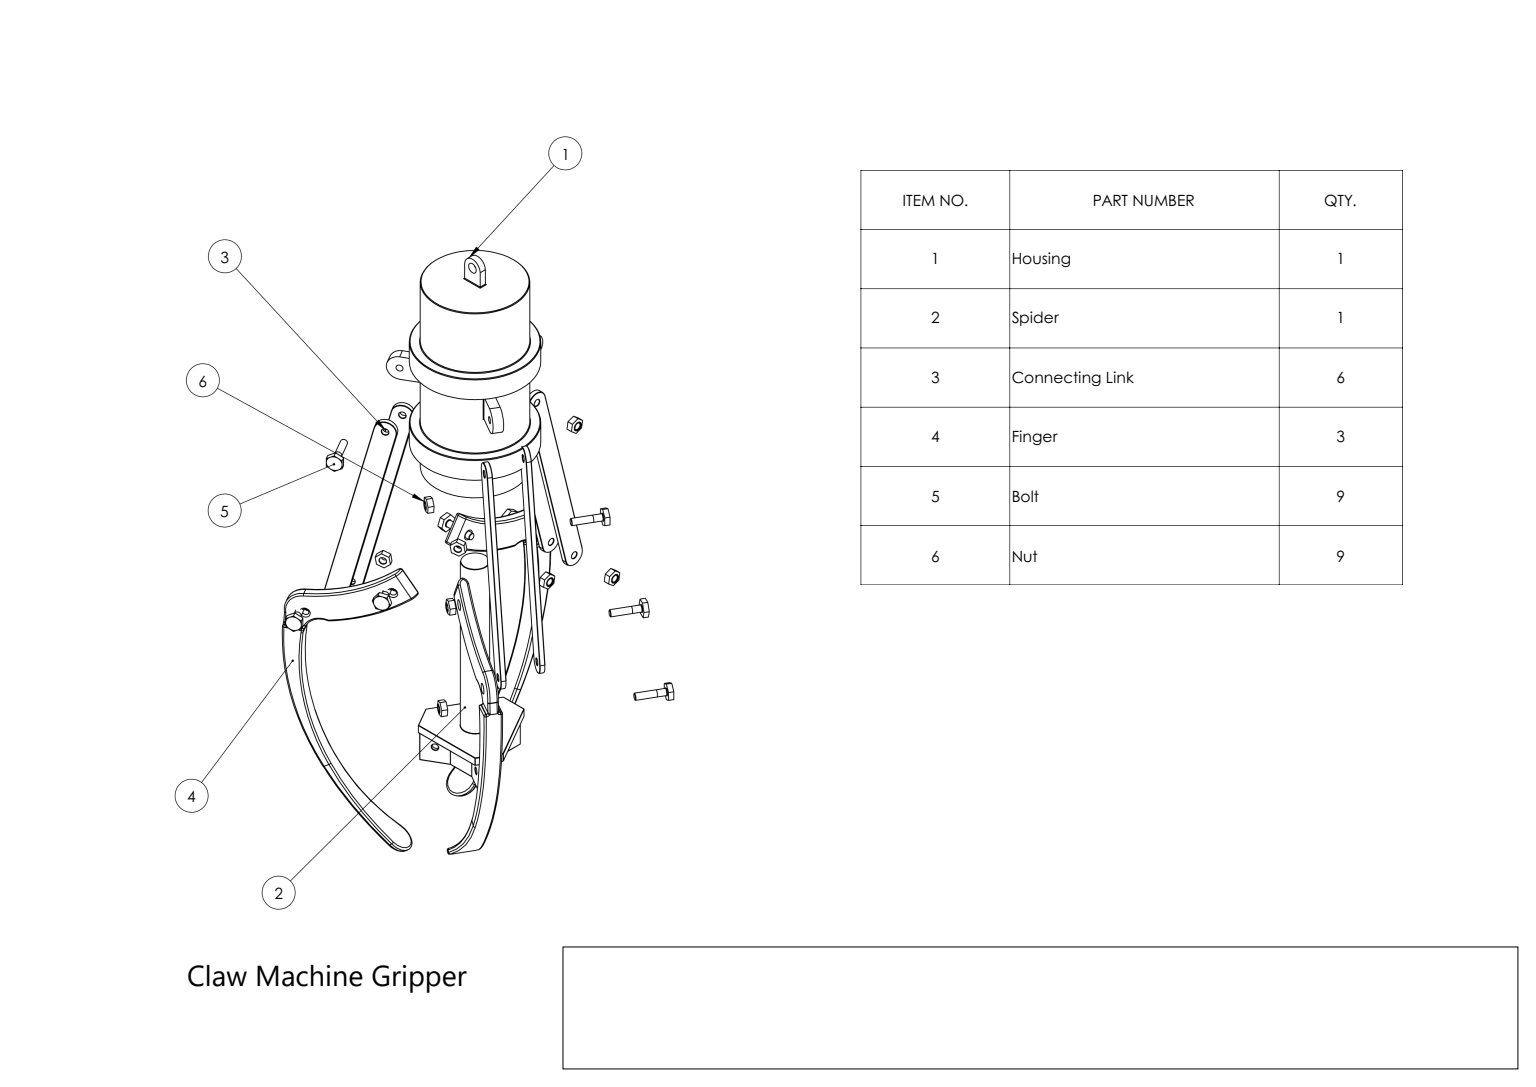
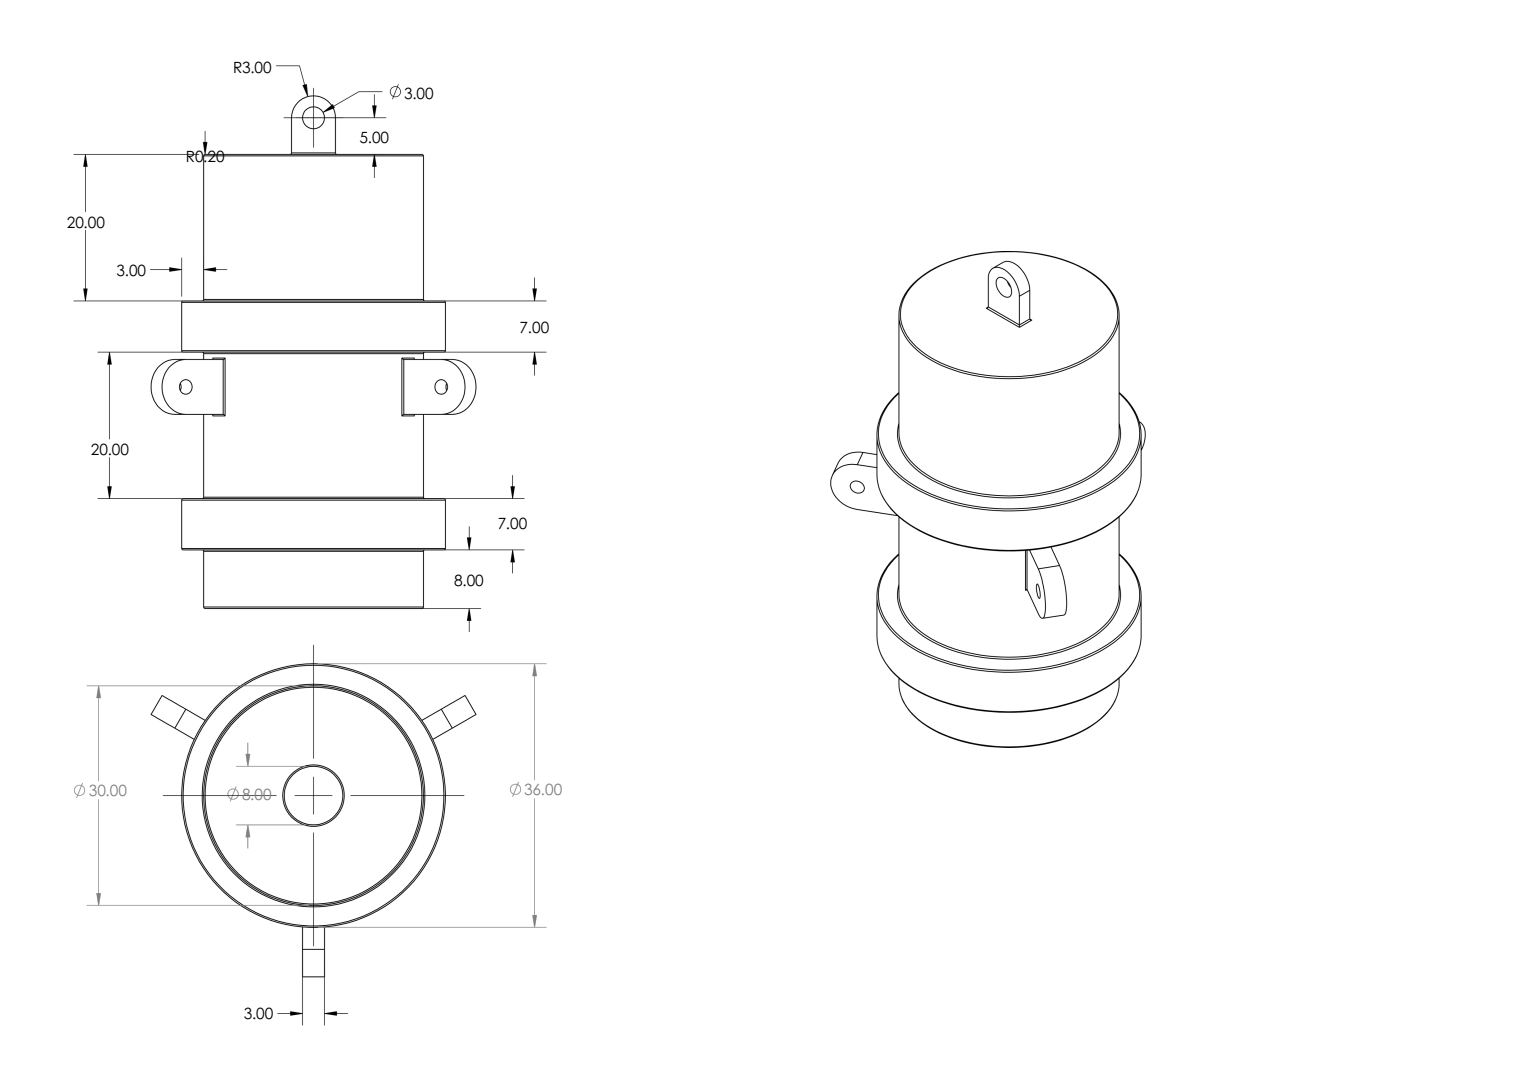
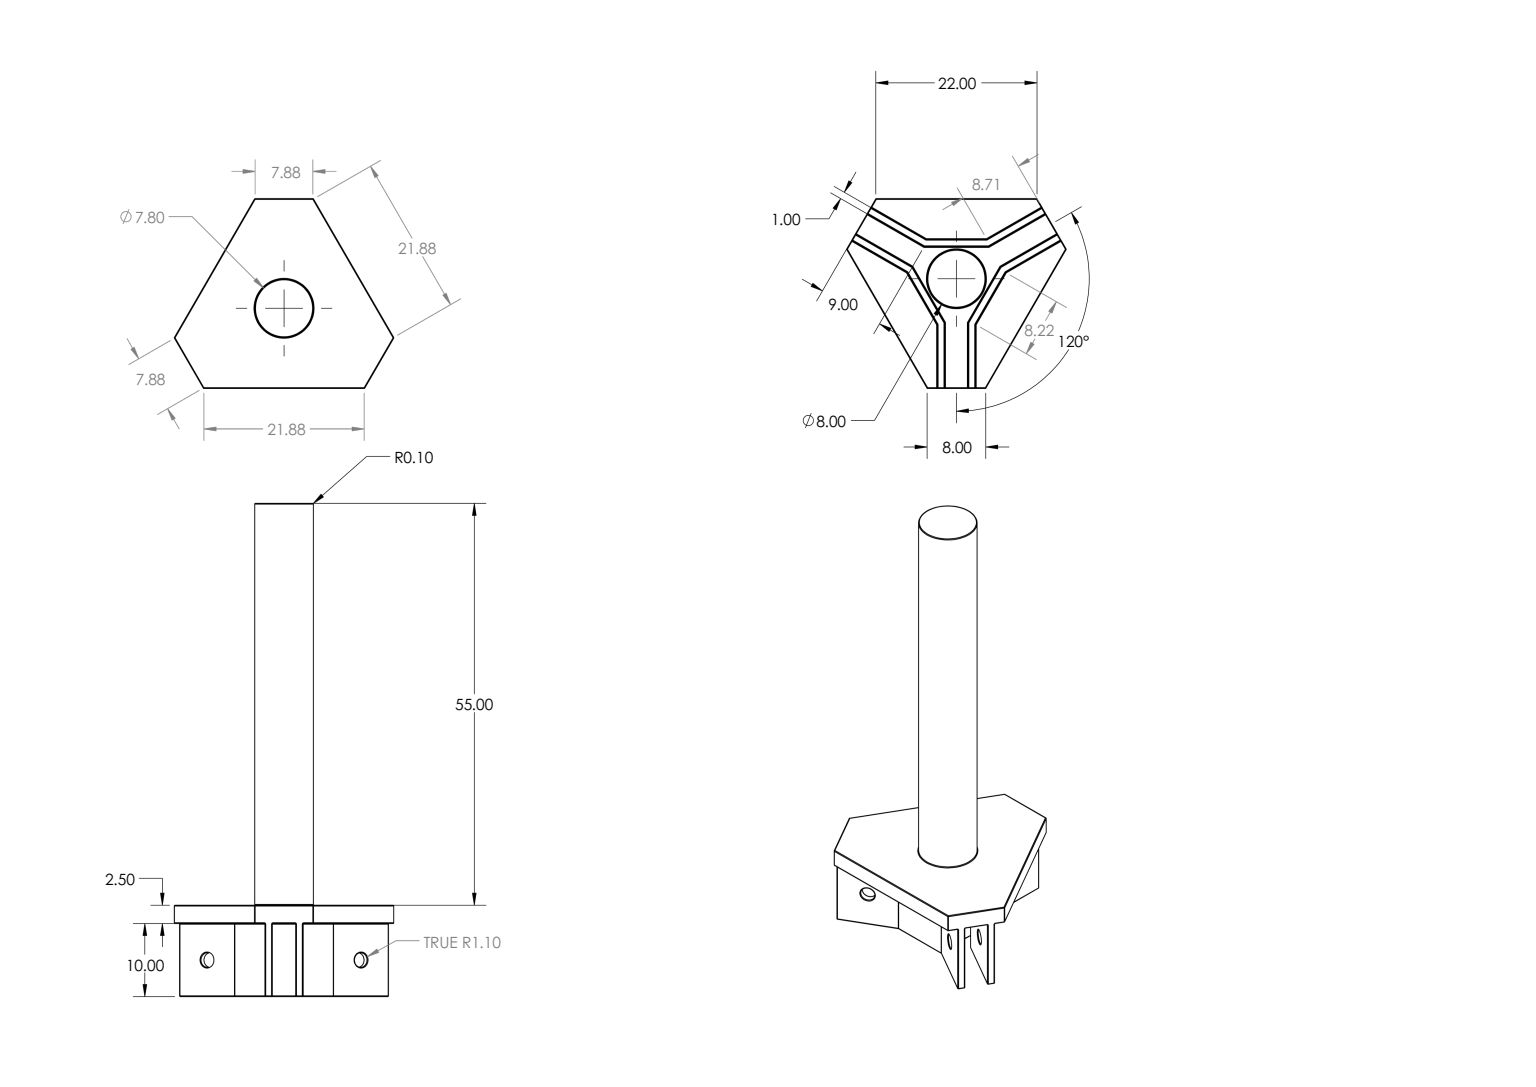
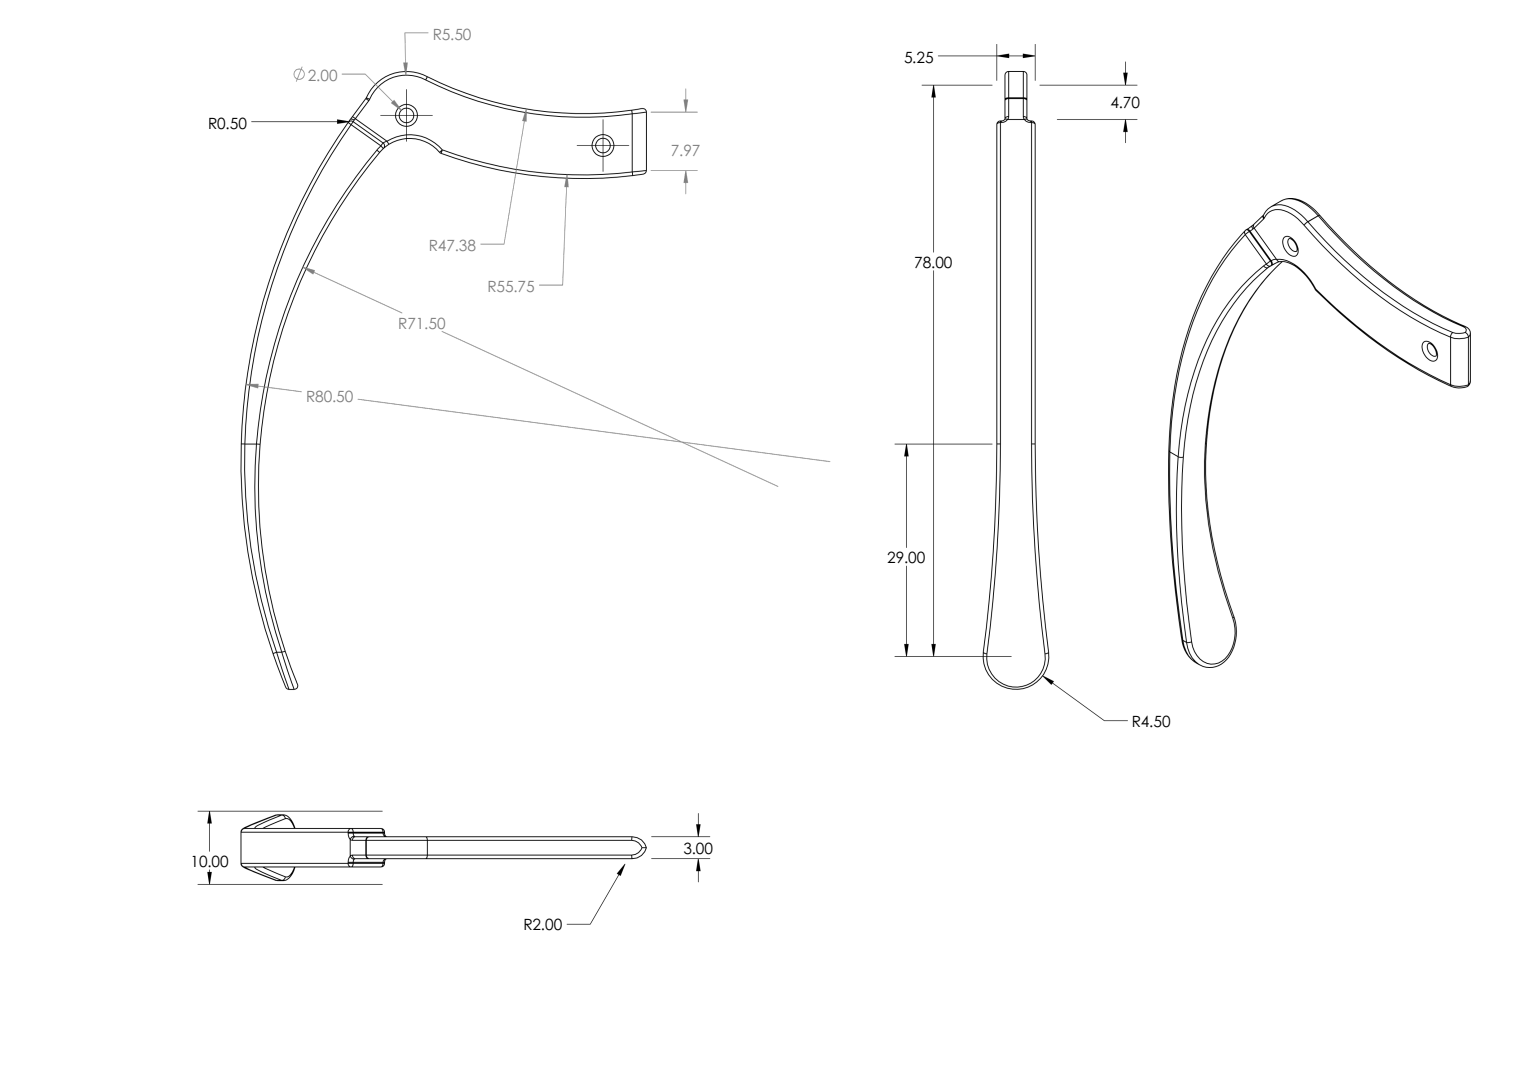
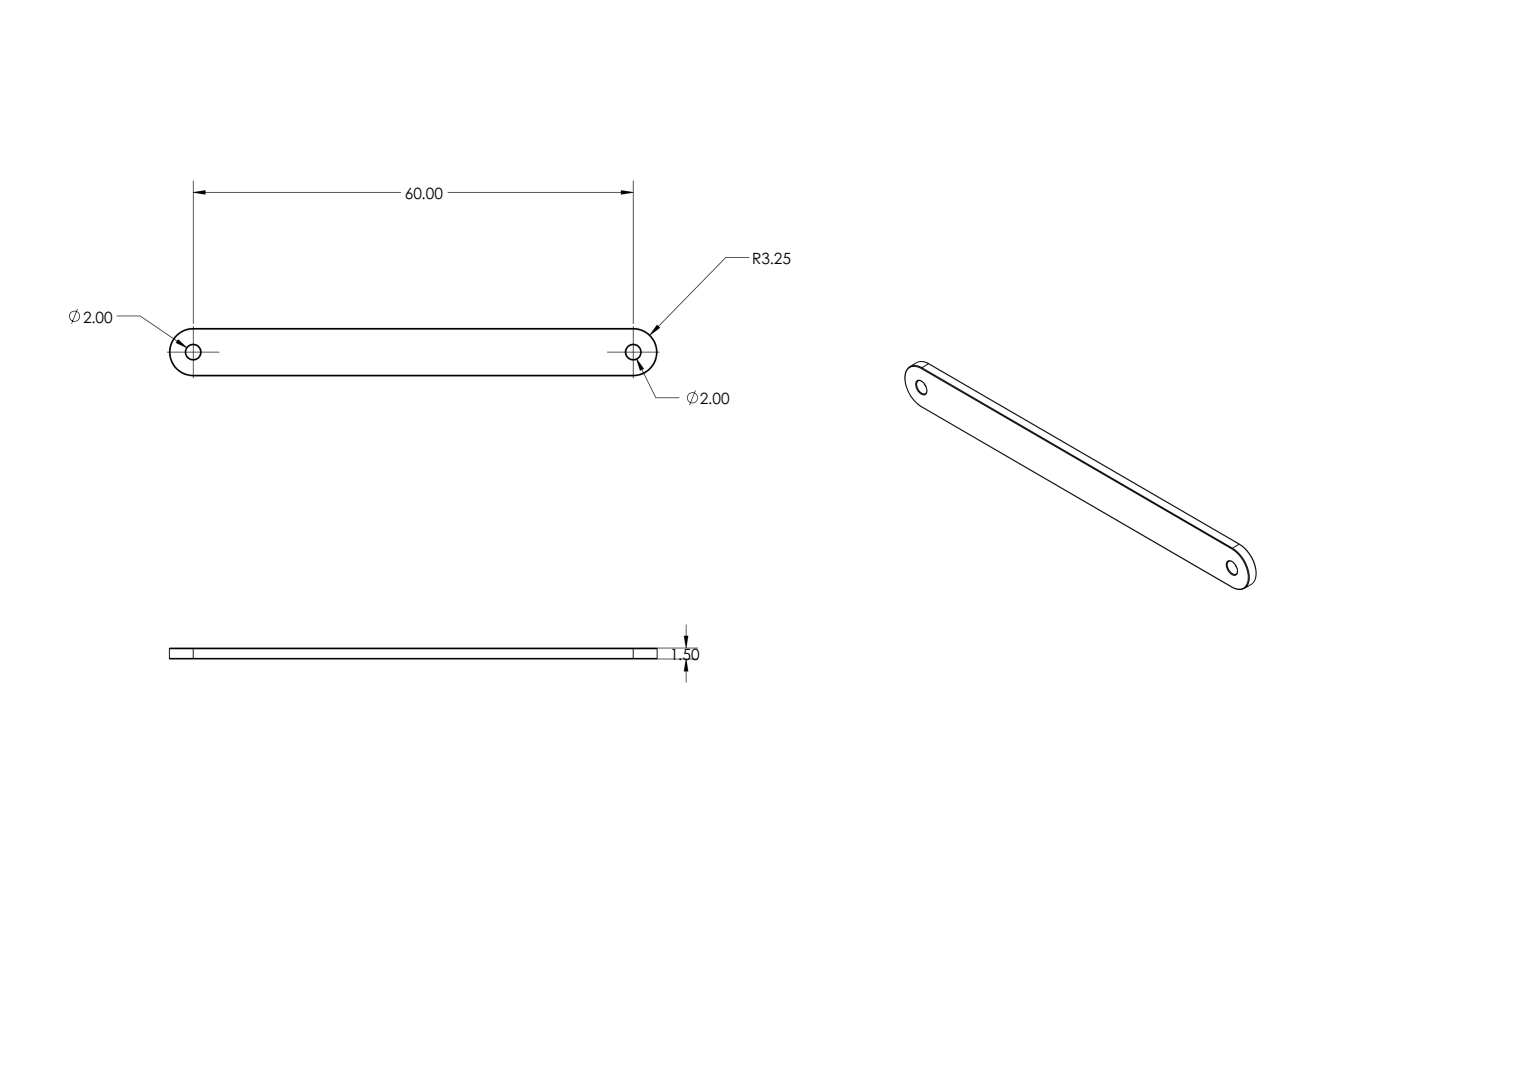
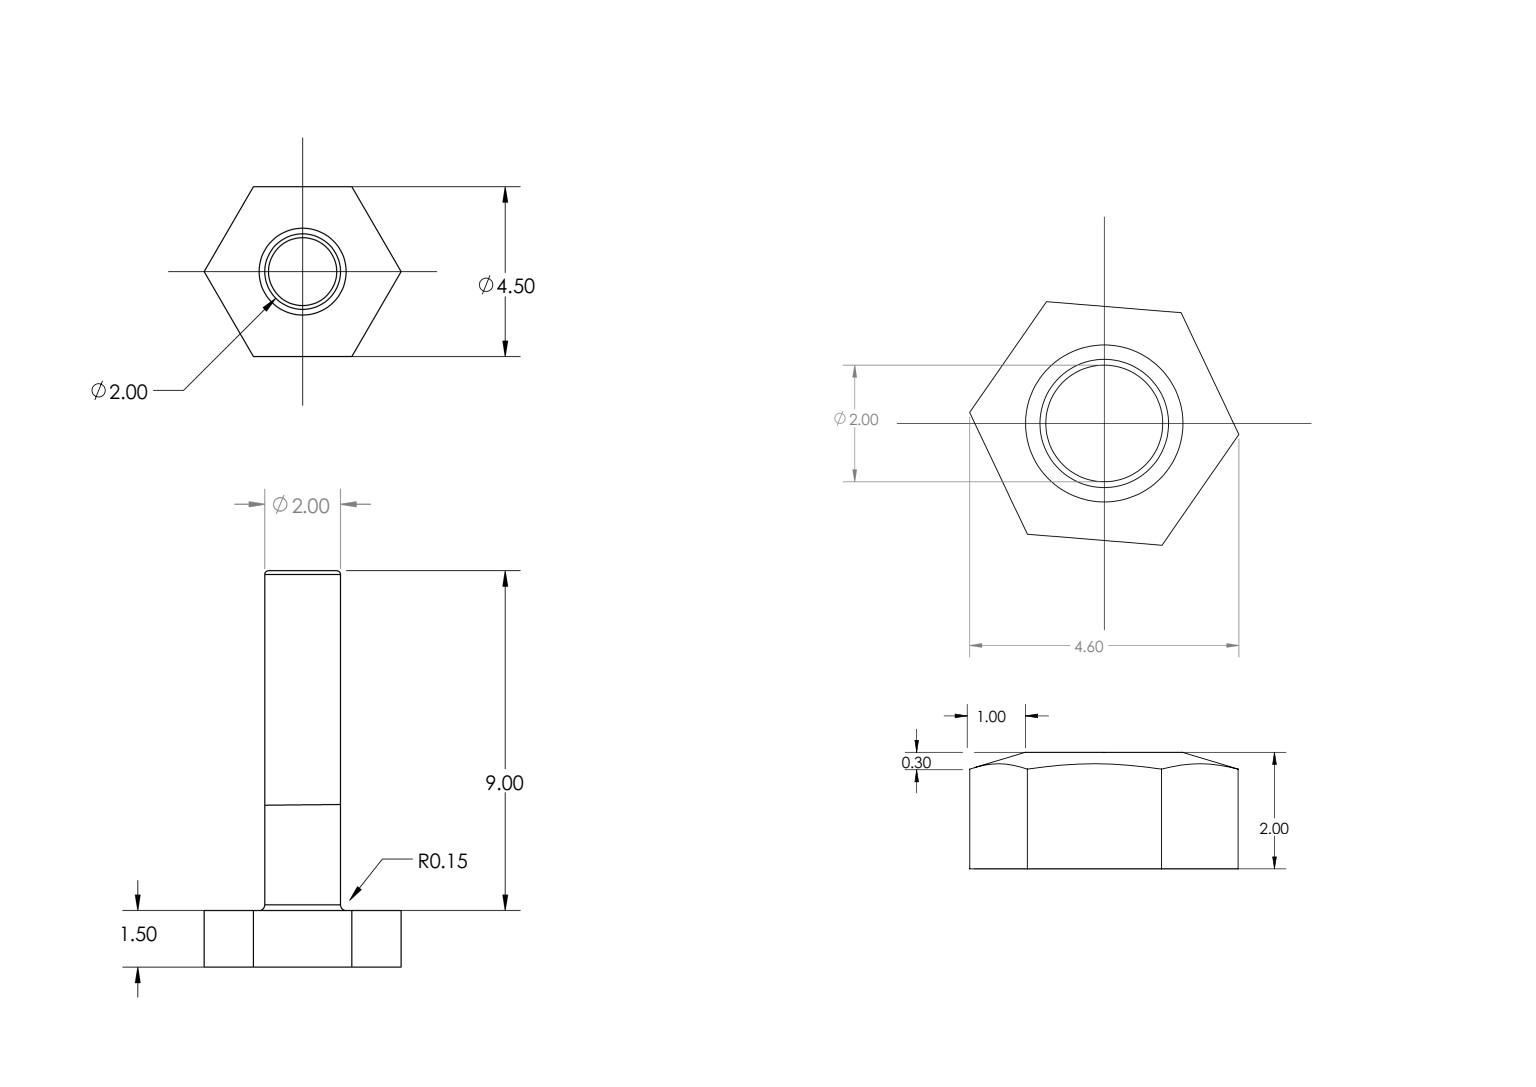
ISO-10303-21;
HEADER;
FILE_DESCRIPTION (('STEP AP214'),
    '1' );
FILE_NAME ('MAT-022',
    '2026-10-24T18:16:00',
    ( '' ),
    ( '' ),
    'SwSTEP 2.0',
    'SolidWorks 2025',
    '' );
FILE_SCHEMA (( 'AUTOMOTIVE_DESIGN' ));
ENDSEC;

DATA;
#1 = CARTESIAN_POINT ( 'NONE',  ( -1.293236445124221312, 0.1355266887446167634, -0.03937007874015747977 ) ) ;
#2 = ORIENTED_EDGE ( 'NONE', *, *, #580, .T. ) ;
#3 = DIRECTION ( 'NONE',  ( 0.000000000000000000, 1.000000000000000000, 0.000000000000000000 ) ) ;
#4 = EDGE_CURVE ( 'NONE', #13144, #1499, #258, .T. ) ;
#5 = CARTESIAN_POINT ( 'NONE',  ( 0.5595825771504284729, -0.1023622047244094474, 0.2048774586467246028 ) ) ;
#6 = DIRECTION ( 'NONE',  ( 0.000000000000000000, 0.000000000000000000, 1.000000000000000000 ) ) ;
#7 = EDGE_LOOP ( 'NONE', ( #10556, #3231, #5022, #13216 ) ) ;
#8 = VERTEX_POINT ( 'NONE', #4783 ) ;
#9 = EDGE_LOOP ( 'NONE', ( #10778, #398, #8347, #5779 ) ) ;
#10 = DIRECTION ( 'NONE',  ( -1.000000000000000000, 0.000000000000000000, 0.000000000000000000 ) ) ;
#11 = LINE ( 'NONE', #8523, #4655 ) ;
#12 = CARTESIAN_POINT ( 'NONE',  ( -1.955186753849255776, -2.907980768360570067, -0.09148540428083716536 ) ) ;
#13 = DIRECTION ( 'NONE',  ( -1.000000000000000000, 0.000000000000000000, 0.000000000000000000 ) ) ;
#14 = LINE ( 'NONE', #82, #14399 ) ;
#15 = CARTESIAN_POINT ( 'NONE',  ( -0.2742631158500640209, -0.2952755905511811885, 0.2765435766697811881 ) ) ;
#16 = CARTESIAN_POINT ( 'NONE',  ( -1.584115185264708403, 0.1296286773226380251, 0.03937007874015747977 ) ) ;
#17 = ORIENTED_EDGE ( 'NONE', *, *, #14890, .T. ) ;
#18 = CARTESIAN_POINT ( 'NONE',  ( -1.944256225378947711, -2.934796208935224637, 0.02867658400294463561 ) ) ;
#19 = CARTESIAN_POINT ( 'NONE',  ( 0.4625984251968510708, -0.1023622047244094474, 0.3807329531073309070 ) ) ;
#20 = DIRECTION ( 'NONE',  ( -0.000000000000000000, -0.000000000000000000, -1.000000000000000000 ) ) ;
#21 = CARTESIAN_POINT ( 'NONE',  ( -1.599581448071076606, 0.1086921510886041942, 0.04859056056449020944 ) ) ;
#22 = ORIENTED_EDGE ( 'NONE', *, *, #7341, .F. ) ;
#23 = ADVANCED_FACE ( 'NONE', ( #187 ), #12882, .T. ) ;
#24 = ORIENTED_EDGE ( 'NONE', *, *, #10025, .F. ) ;
#25 = VERTEX_POINT ( 'NONE', #9568 ) ;
#26 = DIRECTION ( 'NONE',  ( 1.000000000000000000, 0.000000000000000000, 0.000000000000000000 ) ) ;
#27 = LINE ( 'NONE', #5793, #612 ) ;
#28 = DIRECTION ( 'NONE',  ( 1.000000000000000000, 0.000000000000000000, 0.000000000000000000 ) ) ;
#29 = CONTEXT_DEPENDENT_SHAPE_REPRESENTATION ( #6777, #4671 ) ;
#30 = CARTESIAN_POINT ( 'NONE',  ( -0.7455328141524870667, 1.338582677165354395, 0.3622425942647020669 ) ) ;
#31 = CARTESIAN_POINT ( 'NONE',  ( -1.181102362204724310, 0.000000000000000000, 0.02952755905511811330 ) ) ;
#32 = ORIENTED_EDGE ( 'NONE', *, *, #5752, .F. ) ;
#33 = CARTESIAN_POINT ( 'NONE',  ( -0.5905511811023629321, -0.09448818897637796532, 0.1591122789105256785 ) ) ;
#34 = PLANE ( 'NONE',  #8140 ) ;
#35 = CARTESIAN_POINT ( 'NONE',  ( -1.352291563234457650, 0.1355266887446167634, -0.05905511811023622659 ) ) ;
#36 = EDGE_CURVE ( 'NONE', #8997, #3695, #14891, .T. ) ;
#37 = FACE_OUTER_BOUND ( 'NONE', #11677, .T. ) ;
#38 = EDGE_LOOP ( 'NONE', ( #10279, #15210, #1798, #2256 ) ) ;
#39 = EDGE_CURVE ( 'NONE', #10242, #2574, #9139, .T. ) ;
#40 = ORIENTED_EDGE ( 'NONE', *, *, #8775, .T. ) ;
#41 = ORIENTED_EDGE ( 'NONE', *, *, #6196, .F. ) ;
#42 = ORIENTED_EDGE ( 'NONE', *, *, #10757, .F. ) ;
#43 = CARTESIAN_POINT ( 'NONE',  ( -1.592395536721568750, 0.1185427911281754926, -0.04121422034918896526 ) ) ;
#44 = DIRECTION ( 'NONE',  ( 0.000000000000000000, 1.000000000000000000, 0.000000000000000000 ) ) ;
#45 = CARTESIAN_POINT ( 'NONE',  ( -0.05905511811023625435, 2.637795275590551825, 0.03937007874015747977 ) ) ;
#46 = CARTESIAN_POINT ( 'NONE',  ( -0.2822405939667335106, 35.52269057325969470, 0.3493403524838400998 ) ) ;
#47 = DIRECTION ( 'NONE',  ( 0.000000000000000000, -1.000000000000000000, 0.000000000000000000 ) ) ;
#48 = CARTESIAN_POINT ( 'NONE',  ( -1.964126537190516331, -2.749515453455444014, -0.1756903148397123138 ) ) ;
#49 = EDGE_CURVE ( 'NONE', #14974, #2230, #10873, .T. ) ;
#50 = DIRECTION ( 'NONE',  ( -0.000000000000000000, -0.000000000000000000, -1.000000000000000000 ) ) ;
#51 = DIRECTION ( 'NONE',  ( 0.8660254037844385966, 0.000000000000000000, 0.5000000000000000000 ) ) ;
#52 = DIRECTION ( 'NONE',  ( 1.000000000000000000, 0.000000000000000000, -0.000000000000000000 ) ) ;
#53 = EDGE_CURVE ( 'NONE', #7634, #4333, #7363, .T. ) ;
#54 = FACE_OUTER_BOUND ( 'NONE', #13817, .T. ) ;
#55 =( LENGTH_UNIT ( ) NAMED_UNIT ( * ) SI_UNIT ( $, .METRE. ) );
#56 = ORIENTED_EDGE ( 'NONE', *, *, #1265, .F. ) ;
#57 = ADVANCED_FACE ( 'NONE', ( #7220 ), #9740, .F. ) ;
#58 = ORIENTED_EDGE ( 'NONE', *, *, #10893, .T. ) ;
#59 = EDGE_CURVE ( 'NONE', #1289, #10200, #14345, .T. ) ;
#60 = ORIENTED_EDGE ( 'NONE', *, *, #3949, .F. ) ;
#61 = ORIENTED_EDGE ( 'NONE', *, *, #7248, .T. ) ;
#62 = DIRECTION ( 'NONE',  ( 0.000000000000000000, -1.000000000000000000, 0.000000000000000000 ) ) ;
#63 = DIRECTION ( 'NONE',  ( 0.000000000000000000, 0.000000000000000000, 1.000000000000000000 ) ) ;
#64 = DIRECTION ( 'NONE',  ( 0.000000000000000000, 0.000000000000000000, -1.000000000000000000 ) ) ;
#65 = CARTESIAN_POINT ( 'NONE',  ( 0.000000000000000000, 0.5511811023622046335, 0.5590551181102362266 ) ) ;
#66 = DIRECTION ( 'NONE',  ( 1.000000000000000000, 0.000000000000000000, 0.000000000000000000 ) ) ;
#67 = DIRECTION ( 'NONE',  ( -0.000000000000000000, -1.000000000000000000, -0.000000000000000000 ) ) ;
#68 = ORIENTED_EDGE ( 'NONE', *, *, #14092, .T. ) ;
#69 = LENGTH_MEASURE_WITH_UNIT ( LENGTH_MEASURE( 0.02539999999999999897 ), #11905 );
#70 = CARTESIAN_POINT ( 'NONE',  ( -1.580259682937487753, 0.1018956540318996240, -0.04477369844321320291 ) ) ;
#71 = DIRECTION ( 'NONE',  ( 0.000000000000000000, 0.000000000000000000, 1.000000000000000000 ) ) ;
#72 = DIMENSIONAL_EXPONENTS ( 1.000000000000000000, 0.000000000000000000, 0.000000000000000000, 0.000000000000000000, 0.000000000000000000, 0.000000000000000000, 0.000000000000000000 ) ;
#73 = EDGE_LOOP ( 'NONE', ( #10022, #9333, #9772, #13573 ) ) ;
#74 = ORIENTED_EDGE ( 'NONE', *, *, #4819, .F. ) ;
#75 = ADVANCED_FACE ( 'NONE', ( #9803 ), #2445, .T. ) ;
#76 = ORIENTED_EDGE ( 'NONE', *, *, #1408, .T. ) ;
#77 = EDGE_CURVE ( 'NONE', #14789, #11669, #7447, .T. ) ;
#78 = CARTESIAN_POINT ( 'NONE',  ( -2.156935286759944503, -2.012462723082548699, 0.1097304796145711775 ) ) ;
#79 = EDGE_CURVE ( 'NONE', #10775, #13144, #8127, .T. ) ;
#80 = CARTESIAN_POINT ( 'NONE',  ( -2.755905511811024056, -1.630597114118274238, 0.1033464566929129663 ) ) ;
#81 = CARTESIAN_POINT ( 'NONE',  ( 6.750021727583836750E-17, 1.409448818897637956, 0.5511811023622046335 ) ) ;
#82 = CARTESIAN_POINT ( 'NONE',  ( -0.09061599198715356018, 0.07874015748031495954, -0.007444810018878696839 ) ) ;
#83 = DIRECTION ( 'NONE',  ( 0.000000000000000000, 0.000000000000000000, -1.000000000000000000 ) ) ;
#84 = DIRECTION ( 'NONE',  ( 0.000000000000000000, 0.000000000000000000, 1.000000000000000000 ) ) ;
#85 = CARTESIAN_POINT ( 'NONE',  ( -2.061746446265113608, -2.382934929162861870, 0.1354791600993499601 ) ) ;
#86 = ORIENTED_EDGE ( 'NONE', *, *, #142, .F. ) ;
#87 = CARTESIAN_POINT ( 'NONE',  ( -1.964126537190516997, -2.752050336136266928, -0.1561691687464109024 ) ) ;
#88 = CARTESIAN_POINT ( 'NONE',  ( 1.181102362204724310, 4.044111181948214319E-16, -0.02559055118110236185 ) ) ;
#89 = CARTESIAN_POINT ( 'NONE',  ( -0.07002599089419501988, 0.1451652216336531964, -0.05905511811023623353 ) ) ;
#90 = EDGE_LOOP ( 'NONE', ( #14793, #1805, #11512, #7748 ) ) ;
#91 = ORIENTED_EDGE ( 'NONE', *, *, #2937, .F. ) ;
#92 = CIRCLE ( 'NONE', #4574, 0.01968503937007874335 ) ;
#93 = CIRCLE ( 'NONE', #8836, 0.007874015748031499423 ) ;
#94 = ORIENTED_EDGE ( 'NONE', *, *, #12675, .F. ) ;
#95 = CARTESIAN_POINT ( 'NONE',  ( 0.000000000000000000, 0.3543307086614172485, 0.000000000000000000 ) ) ;
#96 = CARTESIAN_POINT ( 'NONE',  ( 0.000000000000000000, 0.000000000000000000, 0.000000000000000000 ) ) ;
#97 =( REPRESENTATION_RELATIONSHIP ('NONE','NONE', #8904, #12105 ) REPRESENTATION_RELATIONSHIP_WITH_TRANSFORMATION ( #6749 )SHAPE_REPRESENTATION_RELATIONSHIP( ) );
#98 = CARTESIAN_POINT ( 'NONE',  ( -1.411977487489316063, -0.03773484711301355182, 0.05405189641583445226 ) ) ;
#99 = DIRECTION ( 'NONE',  ( 0.000000000000000000, 0.000000000000000000, -1.000000000000000000 ) ) ;
#100 = CARTESIAN_POINT ( 'NONE',  ( -0.04748649982359137017, 0.06963377358818916008, -0.06973926505268103482 ) ) ;
#101 = CIRCLE ( 'NONE', #8849, 0.03937007874015747977 ) ;
#102 = DIRECTION ( 'NONE',  ( -0.000000000000000000, 1.000000000000000000, -0.000000000000000000 ) ) ;
#103 = CIRCLE ( 'NONE', #4332, 0.5905511811023621549 ) ;
#104 = DIRECTION ( 'NONE',  ( 1.000000000000000000, 0.000000000000000000, 0.000000000000000000 ) ) ;
#105 = VERTEX_POINT ( 'NONE', #13088 ) ;
#106 = FACE_OUTER_BOUND ( 'NONE', #1446, .T. ) ;
#107 = AXIS2_PLACEMENT_3D ( 'NONE', #2683, #12082, #8785 ) ;
#108 = CARTESIAN_POINT ( 'NONE',  ( -1.185590517044430081, 0.3351394466080224732, -0.05695402829526142324 ) ) ;
#109 = CARTESIAN_POINT ( 'NONE',  ( -0.07635964791965739462, -0.1878198040935885327, 0.05905511811023622659 ) ) ;
#110 = ORIENTED_EDGE ( 'NONE', *, *, #11508, .F. ) ;
#111 = ORIENTED_EDGE ( 'NONE', *, *, #454, .T. ) ;
#113 = VERTEX_POINT ( 'NONE', #2354 ) ;
#112 = CIRCLE ( 'NONE', #12619, 0.007874015748031449116 ) ;
#114 = AXIS2_PLACEMENT_3D ( 'NONE', #1059, #5812, #13822 ) ;
#115 = VERTEX_POINT ( 'NONE', #10106 ) ;
#116 = EDGE_CURVE ( 'NONE', #14687, #9581, #13722, .T. ) ;
#117 = AXIS2_PLACEMENT_3D ( 'NONE', #2165, #3498, #5743 ) ;
#118 = LINE ( 'NONE', #11058, #11152 ) ;
#119 = AXIS2_PLACEMENT_3D ( 'NONE', #8885, #662, #8010 ) ;
#120 = ADVANCED_FACE ( 'NONE', ( #12541 ), #3452, .F. ) ;
#121 = DIRECTION ( 'NONE',  ( 0.000000000000000000, 0.000000000000000000, 1.000000000000000000 ) ) ;
#122 = B_SPLINE_CURVE_WITH_KNOTS ( 'NONE', 3,
 ( #1208, #10680, #10591, #8541, #2360, #2582, #3476, #7059, #15378, #1126 ),
 .UNSPECIFIED., .F., .F.,
 ( 4, 2, 2, 2, 4 ),
 ( 6.547728381081633163E-06, 0.0002695768667942076403, 0.0005326060052073337261, 0.0007956351436204597578, 0.001058664282033585681 ),
 .UNSPECIFIED. ) ;
#123 = DIRECTION ( 'NONE',  ( -0.000000000000000000, -1.000000000000000000, -0.000000000000000000 ) ) ;
#124 = LINE ( 'NONE', #4886, #11098 ) ;
#125 = CARTESIAN_POINT ( 'NONE',  ( -0.9178799135384568819, 36.23251143493320114, 0.6322246801791264748 ) ) ;
#126 = CARTESIAN_POINT ( 'NONE',  ( -0.5871416322685659717, -0.09448818897637796532, 0.1571437749735178357 ) ) ;
#127 = FACE_OUTER_BOUND ( 'NONE', #1547, .T. ) ;
#128 = EDGE_CURVE ( 'NONE', #7239, #11495, #15042, .T. ) ;
#129 = DIRECTION ( 'NONE',  ( 1.224646799147343593E-16, 0.000000000000000000, -1.000000000000000000 ) ) ;
#130 = DIRECTION ( 'NONE',  ( 0.000000000000000000, 1.000000000000000000, -0.000000000000000000 ) ) ;
#131 = AXIS2_PLACEMENT_3D ( 'NONE', #4870, #14445, #104 ) ;
#132 = CIRCLE ( 'NONE', #8366, 0.003937007874015749712 ) ;
#133 = CIRCLE ( 'NONE', #9633, 0.003937007874015754916 ) ;
#134 = CIRCLE ( 'NONE', #2132, 0.03937007874015751446 ) ;
#135 = CARTESIAN_POINT ( 'NONE',  ( 0.000000000000000000, 1.661417322834646049, 0.000000000000000000 ) ) ;
#136 = FACE_OUTER_BOUND ( 'NONE', #9209, .T. ) ;
#137 = AXIS2_PLACEMENT_3D ( 'NONE', #722, #10110, #6416 ) ;
#138 = ORIENTED_EDGE ( 'NONE', *, *, #12039, .T. ) ;
#139 = CARTESIAN_POINT ( 'NONE',  ( -0.01899774626693613230, 0.1736125314593575386, 0.03244910060855325795 ) ) ;
#140 = ORIENTED_EDGE ( 'NONE', *, *, #3284, .F. ) ;
#141 = EDGE_LOOP ( 'NONE', ( #2502, #1091, #11460, #13655 ) ) ;
#142 = EDGE_CURVE ( 'NONE', #9415, #10116, #8053, .T. ) ;
#143 = CIRCLE ( 'NONE', #6372, 0.03937007874015753528 ) ;
#144 = CIRCLE ( 'NONE', #6605, 3.169291338582677753 ) ;
#145 = EDGE_CURVE ( 'NONE', #9212, #10209, #5623, .T. ) ;
#146 = AXIS2_PLACEMENT_3D ( 'NONE', #6930, #11726, #4572 ) ;
#147 = DIRECTION ( 'NONE',  ( -1.000000000000000000, -0.000000000000000000, -0.000000000000000000 ) ) ;
#148 = DIRECTION ( 'NONE',  ( -0.8660254037844398178, 0.000000000000000000, 0.4999999999999979461 ) ) ;
#149 = CIRCLE ( 'NONE', #5881, 0.003937007874015758385 ) ;
#150 = FACE_OUTER_BOUND ( 'NONE', #4683, .T. ) ;
#151 = EDGE_CURVE ( 'NONE', #15270, #8791, #5117, .T. ) ;
#152 = PLANE ( 'NONE',  #3906 ) ;
#153 = DIRECTION ( 'NONE',  ( -0.5000000000000004441, 2.369676336725577685E-14, -0.8660254037844384856 ) ) ;
#154 = DIRECTION ( 'NONE',  ( -1.000000000000000000, 0.000000000000000000, -3.614007241618347785E-16 ) ) ;
#155 = DIRECTION ( 'NONE',  ( 0.4999999999999922284, -0.000000000000000000, -0.8660254037844430375 ) ) ;
#156 = CARTESIAN_POINT ( 'NONE',  ( -0.2652685895081163259, -0.4881889763779528324, 0.03495519865516327068 ) ) ;
#157 = CARTESIAN_POINT ( 'NONE',  ( -0.1181102362204724532, 2.637795275590551825, 0.03937007874015747977 ) ) ;
#158 = AXIS2_PLACEMENT_3D ( 'NONE', #7725, #15171, #6528 ) ;
#159 = AXIS2_PLACEMENT_3D ( 'NONE', #14084, #3448, #5697 ) ;
#160 = AXIS2_PLACEMENT_3D ( 'NONE', #13660, #12490, #1985 ) ;
#161 = VERTEX_POINT ( 'NONE', #8231 ) ;
#162 = ORIENTED_EDGE ( 'NONE', *, *, #7094, .T. ) ;
#163 = AXIS2_PLACEMENT_3D ( 'NONE', #230, #8581, #13368 ) ;
#164 = ORIENTED_EDGE ( 'NONE', *, *, #13819, .T. ) ;
#165 = EDGE_CURVE ( 'NONE', #4902, #13738, #13884, .T. ) ;
#166 = SPHERICAL_SURFACE ( 'NONE', #13897, 0.01968503937007873988 ) ;
#167 = CARTESIAN_POINT ( 'NONE',  ( -1.576192857444134843, 0.1076040293811589832, 0.06348264010174455019 ) ) ;
#168 = VECTOR ( 'NONE', #5103, 39.37007874015748854 ) ;
#169 = CIRCLE ( 'NONE', #8876, 0.003937007874015758385 ) ;
#170 = DIRECTION ( 'NONE',  ( 0.8660254037844361541, 0.000000000000000000, -0.5000000000000042188 ) ) ;
#171 = EDGE_CURVE ( 'NONE', #11793, #14788, #383, .T. ) ;
#172 = DIRECTION ( 'NONE',  ( 0.000000000000000000, -1.000000000000000000, -0.000000000000000000 ) ) ;
#173 = PLANE ( 'NONE',  #1826 ) ;
#174 = CARTESIAN_POINT ( 'NONE',  ( 0.06012952712669449029, 1.041728495490239714, -0.5902914708161598467 ) ) ;
#175 = CIRCLE ( 'NONE', #5908, 0.01968503937007872948 ) ;
#176 = CARTESIAN_POINT ( 'NONE',  ( -1.892121628034221459, -2.891752770451749388, 0.1316657767305224880 ) ) ;
#177 = ORIENTED_EDGE ( 'NONE', *, *, #4532, .F. ) ;
#178 = CARTESIAN_POINT ( 'NONE',  ( -1.953781456863171062, -2.911486273847457618, 0.08694686177389875092 ) ) ;
#179 = DIRECTION ( 'NONE',  ( 0.000000000000000000, -1.000000000000000000, -0.000000000000000000 ) ) ;
#180 = CARTESIAN_POINT ( 'NONE',  ( 0.5412478373021326616, 1.346456692913385877, 0.2362233606508025163 ) ) ;
#181 = ORIENTED_EDGE ( 'NONE', *, *, #8447, .T. ) ;
#182 = EDGE_CURVE ( 'NONE', #9678, #2117, #12141, .T. ) ;
#183 = ORIENTED_EDGE ( 'NONE', *, *, #1290, .T. ) ;
#184 = VECTOR ( 'NONE', #3800, 39.37007874015748143 ) ;
#185 = ORIENTED_EDGE ( 'NONE', *, *, #10784, .F. ) ;
#186 = AXIS2_PLACEMENT_3D ( 'NONE', #15359, #11769, #5780 ) ;
#187 = FACE_OUTER_BOUND ( 'NONE', #7423, .T. ) ;
#188 = CARTESIAN_POINT ( 'NONE',  ( 0.5452755905511544876, -0.4881889763779528324, 0.2375319020879054499 ) ) ;
#189 = CIRCLE ( 'NONE', #9445, 0.2106299212598415904 ) ;
#190 = CARTESIAN_POINT ( 'NONE',  ( -0.05905511811023622659, 1.043263280880422528, -0.5946706712680680518 ) ) ;
#191 = CARTESIAN_POINT ( 'NONE',  ( -1.293236445124221312, 0.1355266887446167634, 0.03937007874015747977 ) ) ;
#192 = FACE_OUTER_BOUND ( 'NONE', #8001, .T. ) ;
#193 = CARTESIAN_POINT ( 'NONE',  ( 0.03346456692913318126, -0.4881889763779528324, 0.05796233017454787556 ) ) ;
#194 = ORIENTED_EDGE ( 'NONE', *, *, #797, .T. ) ;
#195 = DIRECTION ( 'NONE',  ( 0.000000000000000000, 0.000000000000000000, 1.000000000000000000 ) ) ;
#196 = CARTESIAN_POINT ( 'NONE',  ( -1.084824920504545016E-17, 0.000000000000000000, -0.08858267716535432601 ) ) ;
#197 = DIRECTION ( 'NONE',  ( 0.000000000000000000, -1.000000000000000000, 0.000000000000000000 ) ) ;
#198 = VECTOR ( 'NONE', #7263, 39.37007874015748143 ) ;
#199 = CARTESIAN_POINT ( 'NONE',  ( -0.04290857128006120985, -0.1835146052580345633, 0.05099426193563244558 ) ) ;
#200 = ADVANCED_FACE ( 'NONE', ( #4464 ), #1966, .T. ) ;
#201 = DIRECTION ( 'NONE',  ( 0.000000000000000000, 1.000000000000000000, -4.956352788505160310E-16 ) ) ;
#202 = VECTOR ( 'NONE', #642, 39.37007874015748143 ) ;
#203 = ORIENTED_EDGE ( 'NONE', *, *, #9789, .F. ) ;
#204 = ORIENTED_EDGE ( 'NONE', *, *, #11325, .F. ) ;
#205 = ORIENTED_EDGE ( 'NONE', *, *, #2078, .T. ) ;
#206 = AXIS2_PLACEMENT_3D ( 'NONE', #1865, #6710, #10088 ) ;
#207 = ORIENTED_EDGE ( 'NONE', *, *, #14794, .T. ) ;
#208 = DIRECTION ( 'NONE',  ( 0.000000000000000000, 0.000000000000000000, 1.000000000000000000 ) ) ;
#209 = AXIS2_PLACEMENT_3D ( 'NONE', #893, #5803, #3406 ) ;
#210 = DIRECTION ( 'NONE',  ( 0.000000000000000000, -1.000000000000000000, 0.000000000000000000 ) ) ;
#211 = CARTESIAN_POINT ( 'NONE',  ( 0.000000000000000000, 0.007874015748031480341, 0.000000000000000000 ) ) ;
#212 = CARTESIAN_POINT ( 'NONE',  ( -0.7750603732076079000, 37.37889961492984980, 0.3110993617577548220 ) ) ;
#213 = LENGTH_MEASURE_WITH_UNIT ( LENGTH_MEASURE( 0.02539999999999999897 ), #11062 );
#214 = DIRECTION ( 'NONE',  ( -0.000000000000000000, 0.000000000000000000, 1.000000000000000000 ) ) ;
#215 = DIRECTION ( 'NONE',  ( 0.000000000000000000, -1.000000000000000000, 0.000000000000000000 ) ) ;
#216 = LINE ( 'NONE', #1526, #9372 ) ;
#217 = CIRCLE ( 'NONE', #10951, 0.01968503937007873988 ) ;
#218 = CARTESIAN_POINT ( 'NONE',  ( -1.392036056571634317, -0.02280807183030207283, 0.03937007874015747283 ) ) ;
#219 = FACE_OUTER_BOUND ( 'NONE', #2008, .T. ) ;
#220 = VECTOR ( 'NONE', #11691, 39.37007874015748143 ) ;
#221 = EDGE_LOOP ( 'NONE', ( #1582, #15254, #8822, #2376 ) ) ;
#222 = ORIENTED_EDGE ( 'NONE', *, *, #8343, .F. ) ;
#223 = ORIENTED_EDGE ( 'NONE', *, *, #11523, .F. ) ;
#224 = EDGE_CURVE ( 'NONE', #6983, #315, #12637, .T. ) ;
#225 = CIRCLE ( 'NONE', #12233, 0.2303149606299203511 ) ;
#226 = PLANE ( 'NONE',  #15109 ) ;
#227 = CARTESIAN_POINT ( 'NONE',  ( -1.181102362204724310, 0.000000000000000000, 0.02952755905511811330 ) ) ;
#228 = VECTOR ( 'NONE', #10852, 39.37007874015748854 ) ;
#229 = CARTESIAN_POINT ( 'NONE',  ( -0.2359202325321149429, -0.4881889763779528324, 0.06286251073437545966 ) ) ;
#230 = CARTESIAN_POINT ( 'NONE',  ( 0.000000000000000000, 1.622047244094488638, 0.000000000000000000 ) ) ;
#231 = CARTESIAN_POINT ( 'NONE',  ( 0.000000000000000000, 1.035433070866142113, 0.000000000000000000 ) ) ;
#232 = DIRECTION ( 'NONE',  ( 0.000000000000000000, 0.000000000000000000, 1.000000000000000000 ) ) ;
#233 = CARTESIAN_POINT ( 'NONE',  ( 0.05905511811023622659, 1.338626482899105241, -0.5946706712680680518 ) ) ;
#234 = CARTESIAN_POINT ( 'NONE',  ( 0.3944453183761336135, -0.2952755905511811330, 0.1549960689574419737 ) ) ;
#235 = EDGE_CURVE ( 'NONE', #15025, #13855, #13405, .T. ) ;
#236 = ORIENTED_EDGE ( 'NONE', *, *, #15238, .T. ) ;
#237 = ORIENTED_EDGE ( 'NONE', *, *, #13998, .T. ) ;
#238 = VERTEX_POINT ( 'NONE', #12837 ) ;
#239 = ORIENTED_EDGE ( 'NONE', *, *, #11299, .T. ) ;
#240 = ADVANCED_FACE ( 'NONE', ( #9406, #9315 ), #14182, .F. ) ;
#241 = VERTEX_POINT ( 'NONE', #12928 ) ;
#242 = DIRECTION ( 'NONE',  ( 0.5000000000000000000, 0.000000000000000000, 0.8660254037844388186 ) ) ;
#243 = CARTESIAN_POINT ( 'NONE',  ( -0.1618514667033796040, -0.4881889763779528324, 0.2161887458866224576 ) ) ;
#244 = CARTESIAN_POINT ( 'NONE',  ( -0.07022707542947252690, -0.1870727099175784891, -0.03937007874015747283 ) ) ;
#245 = CARTESIAN_POINT ( 'NONE',  ( -2.119441840507266139, -2.390209328812086031, 0.1345547373476347619 ) ) ;
#246 = CARTESIAN_POINT ( 'NONE',  ( -0.1552072824047652788, -0.09448818897637796532, -0.5870514566507987197 ) ) ;
#247 = CARTESIAN_POINT ( 'NONE',  ( -1.909668712890198128, -2.916752030038837873, 0.1028102154675972768 ) ) ;
#248 = ORIENTED_EDGE ( 'NONE', *, *, #12383, .F. ) ;
#249 = DIRECTION ( 'NONE',  ( 0.000000000000000000, 0.000000000000000000, 1.000000000000000000 ) ) ;
#250 = ADVANCED_FACE ( 'NONE', ( #14021 ), #3364, .F. ) ;
#251 = CARTESIAN_POINT ( 'NONE',  ( -0.1552072824047652788, -0.09448818897637796532, -0.5909884645248143498 ) ) ;
#252 = EDGE_CURVE ( 'NONE', #9167, #12754, #13947, .T. ) ;
#253 = VERTEX_POINT ( 'NONE', #4379 ) ;
#254 = ORIENTED_EDGE ( 'NONE', *, *, #8368, .F. ) ;
#255 = ADVANCED_FACE ( 'NONE', ( #3218 ), #9172, .F. ) ;
#256 = EDGE_CURVE ( 'NONE', #14594, #6947, #2197, .T. ) ;
#257 = ORIENTED_EDGE ( 'NONE', *, *, #3314, .T. ) ;
#258 = LINE ( 'NONE', #1429, #5603 ) ;
#259 = FACE_OUTER_BOUND ( 'NONE', #15085, .T. ) ;
#260 = EDGE_CURVE ( 'NONE', #5799, #11532, #7989, .T. ) ;
#261 = CARTESIAN_POINT ( 'NONE',  ( -2.755905511811024056, -1.630597114118275348, -8.792486876640390747 ) ) ;
#262 = DIRECTION ( 'NONE',  ( 2.168404344971007142E-16, 0.000000000000000000, -1.000000000000000000 ) ) ;
#263 = CARTESIAN_POINT ( 'NONE',  ( -0.07545607570875818848, 0.1645859079935991787, -0.03937007874015747977 ) ) ;
#264 = ORIENTED_EDGE ( 'NONE', *, *, #12028, .T. ) ;
#265 = CARTESIAN_POINT ( 'NONE',  ( -1.574484809660039453, 0.1100025355994339177, -0.06175692796179814426 ) ) ;
#266 = CARTESIAN_POINT ( 'NONE',  ( -0.6241293575972478580, -0.2952755905511811330, -0.3215685141414794113 ) ) ;
#267 = DIRECTION ( 'NONE',  ( -0.000000000000000000, -1.000000000000000000, -0.000000000000000000 ) ) ;
#268 = B_SPLINE_CURVE_WITH_KNOTS ( 'NONE', 3,
 ( #14257, #2333, #15438, #8372 ),
 .UNSPECIFIED., .F., .F.,
 ( 4, 4 ),
 ( 0.000000000000000000, 0.0006039794861555876143 ),
 .UNSPECIFIED. ) ;
#269 = PLANE ( 'NONE',  #3681 ) ;
#270 = ORIENTED_EDGE ( 'NONE', *, *, #3011, .T. ) ;
#271 = EDGE_CURVE ( 'NONE', #2172, #6534, #268, .T. ) ;
#272 = ORIENTED_EDGE ( 'NONE', *, *, #5675, .F. ) ;
#273 = EDGE_LOOP ( 'NONE', ( #11844, #14325 ) ) ;
#274 = CARTESIAN_POINT ( 'NONE',  ( -0.4803149606299220720, -0.1023622047244094474, 0.3500470136031578194 ) ) ;
#275 = CARTESIAN_POINT ( 'NONE',  ( 0.5905511811023622659, -0.2952755905511811330, -0.3797276218561363992 ) ) ;
#276 = EDGE_CURVE ( 'NONE', #15338, #8722, #1320, .T. ) ;
#277 = EDGE_CURVE ( 'NONE', #7744, #713, #1617, .T. ) ;
#278 = FACE_OUTER_BOUND ( 'NONE', #9293, .T. ) ;
#279 = DIRECTION ( 'NONE',  ( -0.000000000000000000, 1.000000000000000000, 0.000000000000000000 ) ) ;
#280 = DIRECTION ( 'NONE',  ( -0.8561356751019388867, -0.1506948608623633890, -0.4942901624829493246 ) ) ;
#281 = DIRECTION ( 'NONE',  ( 0.4999999999999966693, 0.000000000000000000, 0.8660254037844405950 ) ) ;
#282 = CARTESIAN_POINT ( 'NONE',  ( -0.1552072824047652788, -0.003937007874015747977, -0.5870514566507987197 ) ) ;
#283 = CARTESIAN_POINT ( 'NONE',  ( -1.596293587998474317, 0.1133155780026106618, 0.1968503937007874127 ) ) ;
#284 = DIRECTION ( 'NONE',  ( -0.4999999999999873990, 0.000000000000000000, 0.8660254037844459241 ) ) ;
#285 = CARTESIAN_POINT ( 'NONE',  ( 0.1552072824047652233, -0.09448818897637796532, -0.5870514566507987197 ) ) ;
#286 = ORIENTED_EDGE ( 'NONE', *, *, #10985, .F. ) ;
#287 = EDGE_LOOP ( 'NONE', ( #11579, #13812, #203, #3433 ) ) ;
#288 = VERTEX_POINT ( 'NONE', #4991 ) ;
#289 = CARTESIAN_POINT ( 'NONE',  ( -2.024460782843922058, -2.569698609574572856, -0.1523405278397521878 ) ) ;
#290 = CARTESIAN_POINT ( 'NONE',  ( -1.943748422590784841, -2.936027745407755685, -0.02327475659521720600 ) ) ;
#291 = DIRECTION ( 'NONE',  ( -0.000000000000000000, -0.000000000000000000, -1.000000000000000000 ) ) ;
#292 = DIRECTION ( 'NONE',  ( 0.000000000000000000, 1.000000000000000000, 9.367506770274758310E-14 ) ) ;
#293 = DIRECTION ( 'NONE',  ( 0.5000000000000035527, 0.000000000000000000, -0.8660254037844365982 ) ) ;
#294 = FACE_OUTER_BOUND ( 'NONE', #5000, .T. ) ;
#295 = PLANE ( 'NONE',  #11664 ) ;
#296 = CARTESIAN_POINT ( 'NONE',  ( -1.908307771495521443, -2.849947446465292522, 0.1332780079517500438 ) ) ;
#297 = CARTESIAN_POINT ( 'NONE',  ( -0.4296613173079366632, 0.000000000000000000, 0.4299076816772784415 ) ) ;
#298 = DIRECTION ( 'NONE',  ( 0.000000000000000000, 0.000000000000000000, 1.000000000000000000 ) ) ;
#299 = EDGE_LOOP ( 'NONE', ( #6916, #11845, #7301, #272 ) ) ;
#300 = ORIENTED_EDGE ( 'NONE', *, *, #2278, .F. ) ;
#301 = ORIENTED_EDGE ( 'NONE', *, *, #11469, .F. ) ;
#302 = ORIENTED_EDGE ( 'NONE', *, *, #9316, .F. ) ;
#303 =( REPRESENTATION_RELATIONSHIP ('NONE','NONE', #8904, #7785 ) REPRESENTATION_RELATIONSHIP_WITH_TRANSFORMATION ( #9745 )SHAPE_REPRESENTATION_RELATIONSHIP( ) );
#304 = ORIENTED_EDGE ( 'NONE', *, *, #14593, .F. ) ;
#305 = DIRECTION ( 'NONE',  ( -3.942553354492736135E-16, 0.000000000000000000, 1.000000000000000000 ) ) ;
#306 = ADVANCED_FACE ( 'NONE', ( #3682 ), #9787, .F. ) ;
#307 = FACE_OUTER_BOUND ( 'NONE', #9651, .T. ) ;
#308 = EDGE_CURVE ( 'NONE', #556, #11529, #4863, .T. ) ;
#309 = PRODUCT ( 'Housing', 'Housing', '', ( #13499 ) ) ;
#310 = DIRECTION ( 'NONE',  ( -0.000000000000000000, 0.000000000000000000, 1.000000000000000000 ) ) ;
#311 = CARTESIAN_POINT ( 'NONE',  ( -0.5871416322685660827, 0.000000000000000000, 0.1610807828475335768 ) ) ;
#312 = CARTESIAN_POINT ( 'NONE',  ( 0.000000000000000000, 1.370078740157480546, 0.000000000000000000 ) ) ;
#313 = DIRECTION ( 'NONE',  ( 0.000000000000000000, 0.000000000000000000, 1.000000000000000000 ) ) ;
#314 = CARTESIAN_POINT ( 'NONE',  ( -1.878928142437690685, -2.924394872804905621, 0.09130279448639455619 ) ) ;
#315 = VERTEX_POINT ( 'NONE', #4702 ) ;
#316 = DIRECTION ( 'NONE',  ( -0.000000000000000000, -0.000000000000000000, -1.000000000000000000 ) ) ;
#317 = EDGE_CURVE ( 'NONE', #12712, #11793, #134, .T. ) ;
#318 = CARTESIAN_POINT ( 'NONE',  ( -1.596030944582886857, 0.1136756404968294887, 0.04477369844403809168 ) ) ;
#319 = CARTESIAN_POINT ( 'NONE',  ( 1.181102362204724310, 4.044111181948214319E-16, 0.02559055118110236185 ) ) ;
#320 = ORIENTED_EDGE ( 'NONE', *, *, #11535, .F. ) ;
#321 = EDGE_LOOP ( 'NONE', ( #11036, #7032, #11996, #10788 ) ) ;
#322 = ORIENTED_EDGE ( 'NONE', *, *, #8280, .F. ) ;
#323 = ADVANCED_FACE ( 'NONE', ( #13159, #11998 ), #8458, .F. ) ;
#324 = ADVANCED_FACE ( 'NONE', ( #5851 ), #15138, .T. ) ;
#325 = CARTESIAN_POINT ( 'NONE',  ( 0.7455328141524921737, 1.190944881889763884, 0.3622425942646917418 ) ) ;
#326 = CYLINDRICAL_SURFACE ( 'NONE', #8227, 0.007874015748031516770 ) ;
#327 = DIRECTION ( 'NONE',  ( 0.000000000000000000, -0.000000000000000000, 1.000000000000000000 ) ) ;
#328 = ORIENTED_EDGE ( 'NONE', *, *, #10975, .T. ) ;
#329 = DIRECTION ( 'NONE',  ( 0.5000000000000035527, 0.000000000000000000, -0.8660254037844365982 ) ) ;
#330 = ADVANCED_FACE ( 'NONE', ( #1096 ), #166, .T. ) ;
#331 = CARTESIAN_POINT ( 'NONE',  ( -0.07118569129171407883, 0.07239639532897743091, 0.03365426801084205055 ) ) ;
#332 = DIRECTION ( 'NONE',  ( 1.971276677246368068E-16, 0.000000000000000000, -1.000000000000000000 ) ) ;
#333 = AXIS2_PLACEMENT_3D ( 'NONE', #13224, #2486, #10943 ) ;
#334 = DIRECTION ( 'NONE',  ( 0.4999999999999995004, 0.000000000000000000, 0.8660254037844390407 ) ) ;
#335 = CARTESIAN_POINT ( 'NONE',  ( -0.3635801767928720230, -0.2952755905511811330, 0.2871962198427739366 ) ) ;
#336 = AXIS2_PLACEMENT_3D ( 'NONE', #14534, #4099, #14697 ) ;
#337 = EDGE_LOOP ( 'NONE', ( #12113, #13474, #4533, #12286 ) ) ;
#338 = EDGE_LOOP ( 'NONE', ( #3355, #15265, #8955, #2444 ) ) ;
#339 = ORIENTED_EDGE ( 'NONE', *, *, #9830, .T. ) ;
#340 = DIRECTION ( 'NONE',  ( -0.8660254037844387076, 0.000000000000000000, 0.4999999999999998890 ) ) ;
#341 = CARTESIAN_POINT ( 'NONE',  ( 0.5649606299213149052, -0.1023622047244094474, 0.2034364137499825587 ) ) ;
#342 = VECTOR ( 'NONE', #8477, 39.37007874015748143 ) ;
#343 = CIRCLE ( 'NONE', #10844, 0.03937007874015761855 ) ;
#344 = VECTOR ( 'NONE', #6500, 39.37007874015748143 ) ;
#345 = CARTESIAN_POINT ( 'NONE',  ( -2.058602741089746946, -2.286826958241420016, 0.1276646238208032913 ) ) ;
#346 = DIRECTION ( 'NONE',  ( 0.000000000000000000, 1.000000000000000000, 0.000000000000000000 ) ) ;
#347 = AXIS2_PLACEMENT_3D ( 'NONE', #14818, #13324, #2592 ) ;
#348 = DIRECTION ( 'NONE',  ( -1.249000902703301108E-15, 0.8219459448134285307, -0.5695655044020486724 ) ) ;
#349 = DIRECTION ( 'NONE',  ( 1.000000000000000000, 0.000000000000000000, 0.000000000000000000 ) ) ;
#350 = DIRECTION ( 'NONE',  ( -0.000000000000000000, -1.000000000000000000, -0.000000000000000000 ) ) ;
#351 = DIRECTION ( 'NONE',  ( -0.8660254037844383745, 0.000000000000000000, -0.5000000000000003331 ) ) ;
#352 = EDGE_CURVE ( 'NONE', #10241, #8022, #13137, .T. ) ;
#353 = DIRECTION ( 'NONE',  ( 0.8660254037844383745, 0.000000000000000000, 0.5000000000000005551 ) ) ;
#354 = DIRECTION ( 'NONE',  ( 0.000000000000000000, 1.000000000000000000, -4.956352788505160310E-16 ) ) ;
#355 = AXIS2_PLACEMENT_3D ( 'NONE', #3021, #14778, #12973 ) ;
#356 = VECTOR ( 'NONE', #8199, 39.37007874015748143 ) ;
#357 = EDGE_LOOP ( 'NONE', ( #2575, #14703, #6111, #12477 ) ) ;
#358 = AXIS2_PLACEMENT_3D ( 'NONE', #8652, #13430, #2699 ) ;
#359 = EDGE_CURVE ( 'NONE', #6020, #2868, #2424, .T. ) ;
#360 = AXIS2_PLACEMENT_3D ( 'NONE', #5949, #6017, #3378 ) ;
#361 = ORIENTED_EDGE ( 'NONE', *, *, #5853, .T. ) ;
#362 = VECTOR ( 'NONE', #2138, 39.37007874015748143 ) ;
#363 = ORIENTED_EDGE ( 'NONE', *, *, #11002, .F. ) ;
#364 = DIRECTION ( 'NONE',  ( -1.000000000000000000, 0.000000000000000000, 0.000000000000000000 ) ) ;
#365 = CARTESIAN_POINT ( 'NONE',  ( -1.943201140612624389, -2.937347705060309622, 0.005521057543908070714 ) ) ;
#366 = CIRCLE ( 'NONE', #3856, 0.5984251968503937480 ) ;
#367 = CIRCLE ( 'NONE', #3357, 0.04330708661417329020 ) ;
#368 = DIRECTION ( 'NONE',  ( 1.000000000000000000, 0.000000000000000000, 0.000000000000000000 ) ) ;
#369 = CIRCLE ( 'NONE', #11114, 0.01968503937007875723 ) ;
#370 = LINE ( 'NONE', #13761, #2577 ) ;
#371 = CARTESIAN_POINT ( 'NONE',  ( 0.5084014747882494856, -0.09842519685039370636, 0.2935257283254013583 ) ) ;
#372 = CIRCLE ( 'NONE', #8882, 0.003937007874015724558 ) ;
#373 = AXIS2_PLACEMENT_3D ( 'NONE', #125, #9593, #8423 ) ;
#374 = CARTESIAN_POINT ( 'NONE',  ( -1.879680750885767360, -2.922298882358313588, 0.01177973773464270624 ) ) ;
#375 = CARTESIAN_POINT ( 'NONE',  ( 0.000000000000000000, 1.653543307086614567, 0.000000000000000000 ) ) ;
#376 = DIRECTION ( 'NONE',  ( 0.4999999999999919509, -0.000000000000000000, -0.8660254037844432595 ) ) ;
#377 = ORIENTED_EDGE ( 'NONE', *, *, #13177, .T. ) ;
#378 = EDGE_CURVE ( 'NONE', #10793, #6772, #12896, .T. ) ;
#379 = ORIENTED_EDGE ( 'NONE', *, *, #10742, .T. ) ;
#380 = VECTOR ( 'NONE', #667, 39.37007874015747433 ) ;
#381 = VERTEX_POINT ( 'NONE', #13298 ) ;
#382 = AXIS2_PLACEMENT_3D ( 'NONE', #11155, #12498, #4323 ) ;
#383 = CIRCLE ( 'NONE', #9126, 0.01968503937007875723 ) ;
#384 = ORIENTED_EDGE ( 'NONE', *, *, #12887, .F. ) ;
#385 = ORIENTED_EDGE ( 'NONE', *, *, #15256, .T. ) ;
#386 = AXIS2_PLACEMENT_3D ( 'NONE', #5527, #841, #9620 ) ;
#387 = B_SPLINE_CURVE_WITH_KNOTS ( 'NONE', 3,
 ( #15169, #13044, #14234, #2304, #4431, #9218 ),
 .UNSPECIFIED., .F., .F.,
 ( 4, 2, 4 ),
 ( 0.000000000000000000, 0.0002588876643434665946, 0.0005177753286869331891 ),
 .UNSPECIFIED. ) ;
#388 = CARTESIAN_POINT ( 'NONE',  ( -1.399712685083875030, -0.02644324258679336959, -0.07678689349530590236 ) ) ;
#389 = DIRECTION ( 'NONE',  ( 0.000000000000000000, 0.000000000000000000, 1.000000000000000000 ) ) ;
#390 = CARTESIAN_POINT ( 'NONE',  ( -1.580080891953811628, 0.1020406297922293454, 0.1968503937007874127 ) ) ;
#391 = DIRECTION ( 'NONE',  ( 0.000000000000000000, 0.000000000000000000, -1.000000000000000000 ) ) ;
#392 = DIRECTION ( 'NONE',  ( 0.000000000000000000, -1.000000000000000000, 0.000000000000000000 ) ) ;
#393 = AXIS2_PLACEMENT_3D ( 'NONE', #707, #4367, #10316 ) ;
#394 = CARTESIAN_POINT ( 'NONE',  ( 0.06604848736013260724, 1.035433070866141891, -0.5868460571724354313 ) ) ;
#395 = AXIS2_PLACEMENT_3D ( 'NONE', #14678, #11510, #3210 ) ;
#396 = CARTESIAN_POINT ( 'NONE',  ( -1.871202120571936245, -2.943029077962952211, 0.04801288353396620384 ) ) ;
#397 = AXIS2_PLACEMENT_3D ( 'NONE', #14731, #8601, #305 ) ;
#398 = ORIENTED_EDGE ( 'NONE', *, *, #9450, .T. ) ;
#399 = CARTESIAN_POINT ( 'NONE',  ( -2.188516668597769499, -1.823600774912196520, -0.1033333524236228068 ) ) ;
#400 = AXIS2_PLACEMENT_3D ( 'NONE', #2168, #7172, #1065 ) ;
#401 = FACE_OUTER_BOUND ( 'NONE', #9524, .T. ) ;
#402 = ORIENTED_EDGE ( 'NONE', *, *, #6447, .F. ) ;
#403 = ORIENTED_EDGE ( 'NONE', *, *, #13234, .T. ) ;
#404 = EDGE_CURVE ( 'NONE', #9943, #2172, #9224, .T. ) ;
#406 = ORIENTED_EDGE ( 'NONE', *, *, #14437, .T. ) ;
#405 = AXIS2_PLACEMENT_3D ( 'NONE', #1476, #4981, #10945 ) ;
#407 = AXIS2_PLACEMENT_3D ( 'NONE', #14638, #376, #9781 ) ;
#408 = AXIS2_PLACEMENT_3D ( 'NONE', #9723, #13299, #5940 ) ;
#409 = EDGE_CURVE ( 'NONE', #5520, #2117, #13395, .T. ) ;
#410 = AXIS2_PLACEMENT_3D ( 'NONE', #3499, #8109, #15408 ) ;
#411 = DIRECTION ( 'NONE',  ( -1.000000000000000000, 4.292327424963333000E-16, -5.289613918360294193E-33 ) ) ;
#412 = FACE_OUTER_BOUND ( 'NONE', #5822, .T. ) ;
#413 = SPHERICAL_SURFACE ( 'NONE', #9205, 0.003937007874015747977 ) ;
#414 = DIRECTION ( 'NONE',  ( -0.8660254037844309360, 0.000000000000000000, 0.5000000000000134337 ) ) ;
#415 = ORIENTED_EDGE ( 'NONE', *, *, #6850, .T. ) ;
#416 = CARTESIAN_POINT ( 'NONE',  ( 0.000000000000000000, 0.5984251968503937480, 0.000000000000000000 ) ) ;
#417 = DIRECTION ( 'NONE',  ( 1.000000000000000000, -6.938893903907222856E-15, 0.000000000000000000 ) ) ;
#418 = DIRECTION ( 'NONE',  ( -3.614007241618347785E-16, 0.000000000000000000, 1.000000000000000000 ) ) ;
#419 = CIRCLE ( 'NONE', #3163, 0.5984251968503937480 ) ;
#420 = DIRECTION ( 'NONE',  ( 0.4999999999999922284, -0.000000000000000000, -0.8660254037844430375 ) ) ;
#421 =( CONVERSION_BASED_UNIT ( 'INCH', #12482 ) LENGTH_UNIT ( ) NAMED_UNIT ( #1062 ) );
#422 = EDGE_CURVE ( 'NONE', #6873, #14162, #4769, .T. ) ;
#423 = AXIS2_PLACEMENT_3D ( 'NONE', #12417, #10053, #6511 ) ;
#424 = EDGE_CURVE ( 'NONE', #1254, #2210, #5620, .T. ) ;
#425 = ORIENTED_EDGE ( 'NONE', *, *, #13589, .F. ) ;
#426 = VERTEX_POINT ( 'NONE', #5147 ) ;
#427 = ORIENTED_EDGE ( 'NONE', *, *, #11037, .F. ) ;
#428 = EDGE_CURVE ( 'NONE', #2378, #3129, #9650, .T. ) ;
#429 = DIRECTION ( 'NONE',  ( 0.5000000000000001110, 0.000000000000000000, -0.8660254037844385966 ) ) ;
#430 = CARTESIAN_POINT ( 'NONE',  ( 0.4854723491485768982, 1.043263280880422528, 0.3484785681409844904 ) ) ;
#431 = CIRCLE ( 'NONE', #7921, 0.003937007874015721089 ) ;
#432 = CARTESIAN_POINT ( 'NONE',  ( -2.092239122479251368, -2.009552950301321861, 0.08993382972064449532 ) ) ;
#433 = DIRECTION ( 'NONE',  ( 0.000000000000000000, 0.000000000000000000, -1.000000000000000000 ) ) ;
#434 = DIRECTION ( 'NONE',  ( -0.9999999999999997780, 1.634720119321182277E-15, 3.332327821733210488E-16 ) ) ;
#435 = CARTESIAN_POINT ( 'NONE',  ( -0.4803149606299220720, -0.4881889763779528324, 0.3500470136031578194 ) ) ;
#436 = AXIS2_PLACEMENT_3D ( 'NONE', #8469, #13242, #2503 ) ;
#437 = DIRECTION ( 'NONE',  ( 0.000000000000000000, 0.000000000000000000, -1.000000000000000000 ) ) ;
#438 = CARTESIAN_POINT ( 'NONE',  ( -0.1574803149606299191, -0.09448818897637796532, -0.5909884645248143498 ) ) ;
#439 = CARTESIAN_POINT ( 'NONE',  ( -0.1023622047242991467, -0.4921259842519685179, -0.5909884645248154600 ) ) ;
#440 = AXIS2_PLACEMENT_3D ( 'NONE', #4329, #9129, #13902 ) ;
#441 = CARTESIAN_POINT ( 'NONE',  ( 0.3780663654712341781, -0.2952755905511811330, 0.1046250900831900282 ) ) ;
#442 = ADVANCED_FACE ( 'NONE', ( #5054 ), #14795, .T. ) ;
#443 = DIRECTION ( 'NONE',  ( 0.000000000000000000, 0.000000000000000000, -1.000000000000000000 ) ) ;
#444 = ORIENTED_EDGE ( 'NONE', *, *, #4068, .T. ) ;
#445 = CIRCLE ( 'NONE', #8476, 0.003937007874015749712 ) ;
#446 = AXIS2_PLACEMENT_3D ( 'NONE', #1079, #4450, #2315 ) ;
#447 = EDGE_CURVE ( 'NONE', #12889, #4456, #881, .T. ) ;
#448 = ORIENTED_EDGE ( 'NONE', *, *, #6594, .T. ) ;
#449 = DIRECTION ( 'NONE',  ( -1.000000000000000000, 0.000000000000000000, 0.000000000000000000 ) ) ;
#450 = VERTEX_POINT ( 'NONE', #14958 ) ;
#451 = AXIS2_PLACEMENT_3D ( 'NONE', #1495, #12462, #1728 ) ;
#452 = EDGE_LOOP ( 'NONE', ( #15074, #4990 ) ) ;
#453 = PRODUCT_DEFINITION_SHAPE ( 'NONE', 'NONE',  #15473 ) ;
#454 = EDGE_CURVE ( 'NONE', #4728, #13507, #2390, .T. ) ;
#455 = VECTOR ( 'NONE', #1209, 39.37007874015748143 ) ;
#456 = DIRECTION ( 'NONE',  ( 1.000000000000000000, 0.000000000000000000, 0.000000000000000000 ) ) ;
#457 = CARTESIAN_POINT ( 'NONE',  ( -1.925024858772766745, -2.949472151676825860, -0.01333363273917731115 ) ) ;
#458 = CIRCLE ( 'NONE', #15208, 0.1476377952755906220 ) ;
#459 = CARTESIAN_POINT ( 'NONE',  ( 0.1062992125984796032, -0.4921259842519685179, -0.2482618547481154347 ) ) ;
#460 = ADVANCED_FACE ( 'NONE', ( #13701 ), #4132, .T. ) ;
#461 = FACE_OUTER_BOUND ( 'NONE', #11373, .T. ) ;
#462 = DIRECTION ( 'NONE',  ( 6.484947573745102394E-15, -1.000000000000000000, 2.431855340154413200E-16 ) ) ;
#463 = MECHANICAL_DESIGN_GEOMETRIC_PRESENTATION_REPRESENTATION (  '', ( #2947 ), #13453 ) ;
#464 = CARTESIAN_POINT ( 'NONE',  ( 0.09842519685044814892, -0.2952755905511811330, -0.4190977005962941426 ) ) ;
#465 = CARTESIAN_POINT ( 'NONE',  ( -1.915481817270058729, -2.830827465095222983, -0.1437034448495827788 ) ) ;
#466 = CARTESIAN_POINT ( 'NONE',  ( -2.054789683517501242, -2.568945684013816066, -0.1522427580697401084 ) ) ;
#467 = CARTESIAN_POINT ( 'NONE',  ( -1.276200637803905691, -0.1988000726501942539, 0.08366141732283455257 ) ) ;
#468 = ORIENTED_EDGE ( 'NONE', *, *, #9328, .F. ) ;
#469 = EDGE_LOOP ( 'NONE', ( #58, #3143, #2480, #4682 ) ) ;
#470 = EDGE_LOOP ( 'NONE', ( #2479, #415, #5574, #10167, #3437 ) ) ;
#471 = ORIENTED_EDGE ( 'NONE', *, *, #7915, .F. ) ;
#472 = ADVANCED_FACE ( 'NONE', ( #7735 ), #4183, .T. ) ;
#473 = EDGE_LOOP ( 'NONE', ( #12721, #4306, #12008, #8418 ) ) ;
#474 = CIRCLE ( 'NONE', #9220, 0.003937007874015724558 ) ;
#475 = CARTESIAN_POINT ( 'NONE',  ( -1.409468994508474404, -0.007141353241660916562, -0.06138260383184675206 ) ) ;
#476 = LINE ( 'NONE', #5221, #628 ) ;
#477 = DIRECTION ( 'NONE',  ( 0.000000000000000000, 0.000000000000000000, -1.000000000000000000 ) ) ;
#478 = LINE ( 'NONE', #390, #6847 ) ;
#479 = ADVANCED_FACE ( 'NONE', ( #6538 ), #4638, .T. ) ;
#480 = CARTESIAN_POINT ( 'NONE',  ( 0.000000000000000000, 0.000000000000000000, 0.000000000000000000 ) ) ;
#481 = DIRECTION ( 'NONE',  ( 0.000000000000000000, 0.000000000000000000, 1.000000000000000000 ) ) ;
#482 = VECTOR ( 'NONE', #10408, 39.37007874015748854 ) ;
#483 = CARTESIAN_POINT ( 'NONE',  ( -1.883836775286372056, -2.912146259469937881, -0.05616283913476798756 ) ) ;
#484 = EDGE_LOOP ( 'NONE', ( #14389, #4298, #8359 ) ) ;
#485 = CARTESIAN_POINT ( 'NONE',  ( -2.119441840505075447, -2.390209328808487133, -0.1345547373467393670 ) ) ;
#486 = CARTESIAN_POINT ( 'NONE',  ( -1.234181327013985197, 0.1355266887446167634, -0.03937007874015747977 ) ) ;
#487 = ORIENTED_EDGE ( 'NONE', *, *, #10319, .T. ) ;
#488 = ORIENTED_EDGE ( 'NONE', *, *, #9455, .T. ) ;
#489 = ORIENTED_EDGE ( 'NONE', *, *, #9553, .T. ) ;
#490 = CARTESIAN_POINT ( 'NONE',  ( 0.000000000000000000, 1.035433070866142113, 0.000000000000000000 ) ) ;
#491 = DIRECTION ( 'NONE',  ( 0.000000000000000000, -0.000000000000000000, 1.000000000000000000 ) ) ;
#492 = CARTESIAN_POINT ( 'NONE',  ( -0.4722458785514955237, -0.6629481244416842722, 0.07874015748031495954 ) ) ;
#493 = DIRECTION ( 'NONE',  ( 0.000000000000000000, 0.000000000000000000, -1.000000000000000000 ) ) ;
#494 = FACE_OUTER_BOUND ( 'NONE', #12042, .T. ) ;
#495 = ORIENTED_EDGE ( 'NONE', *, *, #9928, .F. ) ;
#496 = CARTESIAN_POINT ( 'NONE',  ( -1.568343923620152180, 0.1178486908565801600, -0.05905511811023622659 ) ) ;
#497 = CARTESIAN_POINT ( 'NONE',  ( 0.000000000000000000, 0.3228346456692913757, 0.000000000000000000 ) ) ;
#498 = FACE_OUTER_BOUND ( 'NONE', #1145, .T. ) ;
#499 = CARTESIAN_POINT ( 'NONE',  ( -0.5445274672588088505, 1.043263280880422528, 0.2461921031270815630 ) ) ;
#500 = SURFACE_SIDE_STYLE ('',( #733 ) ) ;
#501 = ORIENTED_EDGE ( 'NONE', *, *, #13678, .T. ) ;
#502 = EDGE_LOOP ( 'NONE', ( #12142, #12674, #7426, #14352 ) ) ;
#503 = CARTESIAN_POINT ( 'NONE',  ( 0.000000000000000000, 0.03937007874015749365, 0.000000000000000000 ) ) ;
#504 = DIRECTION ( 'NONE',  ( -1.000000000000000000, 0.000000000000000000, 0.000000000000000000 ) ) ;
#505 = EDGE_CURVE ( 'NONE', #6948, #6036, #613, .T. ) ;
#506 = DIRECTION ( 'NONE',  ( -0.8660254037844385966, 0.000000000000000000, -0.5000000000000001110 ) ) ;
#507 = CYLINDRICAL_SURFACE ( 'NONE', #14125, 0.03937007874015751446 ) ;
#508 = ADVANCED_FACE ( 'NONE', ( #11025 ), #2235, .T. ) ;
#509 = CARTESIAN_POINT ( 'NONE',  ( -0.06692913385815735250, -0.4881889763779528324, -0.5870514566507987197 ) ) ;
#510 = DIRECTION ( 'NONE',  ( 0.4999999999999995004, 0.000000000000000000, 0.8660254037844390407 ) ) ;
#511 = DIRECTION ( 'NONE',  ( 0.000000000000000000, 0.000000000000000000, -1.000000000000000000 ) ) ;
#512 = LINE ( 'NONE', #11478, #1386 ) ;
#513 = EDGE_CURVE ( 'NONE', #14143, #14454, #5809, .T. ) ;
#514 = DIRECTION ( 'NONE',  ( 1.000000000000000000, 0.000000000000000000, 3.075191616504340279E-15 ) ) ;
#515 = ORIENTED_EDGE ( 'NONE', *, *, #13205, .T. ) ;
#516 = ORIENTED_EDGE ( 'NONE', *, *, #6244, .T. ) ;
#517 = VERTEX_POINT ( 'NONE', #10766 ) ;
#518 = ORIENTED_EDGE ( 'NONE', *, *, #11825, .T. ) ;
#519 = PLANE ( 'NONE',  #5081 ) ;
#520 = CARTESIAN_POINT ( 'NONE',  ( -1.945810312050074042, -2.931088922611430281, -0.07891651694308547682 ) ) ;
#521 =( NAMED_UNIT ( * ) PLANE_ANGLE_UNIT ( ) SI_UNIT ( $, .RADIAN. ) );
#522 = EDGE_CURVE ( 'NONE', #14099, #6733, #9902, .T. ) ;
#523 = DIRECTION ( 'NONE',  ( -1.224646799147343593E-16, 0.000000000000000000, -1.000000000000000000 ) ) ;
#524 = CARTESIAN_POINT ( 'NONE',  ( -1.973160353001477185, -2.810434395070632529, -0.1731278957434206622 ) ) ;
#525 = CARTESIAN_POINT ( 'NONE',  ( -1.880200301354544967, -2.921039053327021850, 0.02314659398703503707 ) ) ;
#526 = ADVANCED_FACE ( 'NONE', ( #4500 ), #6362, .T. ) ;
#527 = CYLINDRICAL_SURFACE ( 'NONE', #3584, 0.003937007874015750579 ) ;
#528 = FACE_OUTER_BOUND ( 'NONE', #10014, .T. ) ;
#529 = EDGE_CURVE ( 'NONE', #9431, #11432, #639, .T. ) ;
#530 = EDGE_LOOP ( 'NONE', ( #9699, #86, #11976, #15040 ) ) ;
#531 = ORIENTED_EDGE ( 'NONE', *, *, #11516, .F. ) ;
#532 = VERTEX_POINT ( 'NONE', #9284 ) ;
#533 = ORIENTED_EDGE ( 'NONE', *, *, #2731, .T. ) ;
#534 = ORIENTED_EDGE ( 'NONE', *, *, #10419, .T. ) ;
#535 = DIRECTION ( 'NONE',  ( 0.000000000000000000, 1.000000000000000000, 0.000000000000000000 ) ) ;
#536 = DIRECTION ( 'NONE',  ( 0.000000000000000000, 0.000000000000000000, 1.000000000000000000 ) ) ;
#537 = CARTESIAN_POINT ( 'NONE',  ( -0.5871416322685659717, -0.09448818897637796532, 0.1571437749735178357 ) ) ;
#538 = CARTESIAN_POINT ( 'NONE',  ( -1.511943070284283097, 0.2262540267724839904, -0.05905511811023622659 ) ) ;
#539 = CARTESIAN_POINT ( 'NONE',  ( -1.224409448818897461, 5.303588500244450842E-18, -0.02952755905511811330 ) ) ;
#540 = CYLINDRICAL_SURFACE ( 'NONE', #4641, 0.003937007874015724558 ) ;
#541 = CARTESIAN_POINT ( 'NONE',  ( 0.000000000000000000, 1.653543307086614567, 0.000000000000000000 ) ) ;
#542 = CARTESIAN_POINT ( 'NONE',  ( -1.908381546755280489, -2.920376482534968954, 0.09751899391724366817 ) ) ;
#543 = EDGE_LOOP ( 'NONE', ( #6687, #8996, #6929, #6640, #1120 ) ) ;
#544 = CARTESIAN_POINT ( 'NONE',  ( -2.156938452688012653, -2.012428322113554824, -0.1097289591313703738 ) ) ;
#545 = CARTESIAN_POINT ( 'NONE',  ( 0.000000000000000000, 2.433070866141732846, 0.000000000000000000 ) ) ;
#546 = EDGE_CURVE ( 'NONE', #2999, #877, #1956, .T. ) ;
#547 = CARTESIAN_POINT ( 'NONE',  ( 0.000000000000000000, 0.007874015748031480341, 0.000000000000000000 ) ) ;
#548 = ORIENTED_EDGE ( 'NONE', *, *, #7094, .F. ) ;
#549 = ORIENTED_EDGE ( 'NONE', *, *, #1610, .T. ) ;
#550 = EDGE_CURVE ( 'NONE', #7731, #9204, #1632, .T. ) ;
#551 = ORIENTED_EDGE ( 'NONE', *, *, #10373, .T. ) ;
#552 = CARTESIAN_POINT ( 'NONE',  ( -1.100415514366371639, -0.04998955061625894036, 0.1968503937007874127 ) ) ;
#553 = FACE_OUTER_BOUND ( 'NONE', #4160, .T. ) ;
#554 = CARTESIAN_POINT ( 'NONE',  ( 0.2364476915724980366, -0.4921259842519685179, 0.06377609659104091500 ) ) ;
#555 = CARTESIAN_POINT ( 'NONE',  ( -0.04290857128006120985, -0.1835146052580345633, -0.05099426193563244558 ) ) ;
#556 = VERTEX_POINT ( 'NONE', #12972 ) ;
#557 = CARTESIAN_POINT ( 'NONE',  ( -2.041848724490688216, -2.380718792664717309, 0.1160226956207114496 ) ) ;
#558 = PLANE ( 'NONE',  #8104 ) ;
#559 = DIRECTION ( 'NONE',  ( 0.000000000000000000, 0.000000000000000000, 1.000000000000000000 ) ) ;
#560 = EDGE_LOOP ( 'NONE', ( #8023, #12379, #10629, #7056 ) ) ;
#561 = PRODUCT_DEFINITION ( 'UNKNOWN', '', #4613, #13178 ) ;
#562 = VERTEX_POINT ( 'NONE', #13772 ) ;
#563 = VERTEX_POINT ( 'NONE', #1859 ) ;
#564 =( BOUNDED_SURFACE ( )  B_SPLINE_SURFACE ( 3, 2, ( 
 ( #9561, #13304, #3604 ),
 ( #9494, #8383, #12152 ),
 ( #3458, #10571, #1102 ),
 ( #6014, #3760, #11926 ),
 ( #15444, #10661, #10801 ),
 ( #1193, #13168, #4844 ),
 ( #9649, #14426, #3688 ),
 ( #3529, #13010, #4707 ),
 ( #8466, #8300, #12065 ),
 ( #8529, #7275, #1327 ),
 ( #8236, #6086, #10885 ),
 ( #14188, #176, #2568 ),
 ( #7345, #15356, #3825 ),
 ( #247, #4057, #6241 ),
 ( #542, #2662, #1645 ),
 ( #8609, #314, #8768 ),
 ( #14802, #5293, #13394 ),
 ( #10095, #11196, #7434 ),
 ( #1555, #4143, #5064 ),
 ( #12370, #13537, #4998 ),
 ( #8840, #396, #14882 ),
 ( #2799, #7670, #12295 ),
 ( #6308, #5150, #9870 ),
 ( #14740, #5227, #13710 ),
 ( #7743, #12234, #1493 ),
 ( #11030, #8936, #2975 ),
 ( #7509, #7571, #3917 ),
 ( #14655, #8699, #11104 ),
 ( #2739, #9958, #13473 ),
 ( #6403, #3994, #483 ),
 ( #10021, #13618, #2889 ),
 ( #12460, #1726, #6485 ),
 ( #11270, #1418, #6173 ),
 ( #10965, #9794, #14564 ),
 ( #5615, #13781, #2097 ),
 ( #937, #15191, #6872 ),
 ( #10252, #6714, #11505 ),
 ( #1872, #12604, #11431 ),
 ( #4455, #11667, #11574 ),
 ( #12826, #15264, #9074 ),
 ( #9009, #4220, #4285 ),
 ( #9238, #3350, #14011 ),
 ( #8044, #7901, #2017 ),
 ( #4523, #5529, #5693 ),
 ( #13851, #623, #3273 ),
 ( #9159, #13937, #11341 ) ),
 .UNSPECIFIED., .F., .F., .T. ) 
 B_SPLINE_SURFACE_WITH_KNOTS ( ( 4, 2, 2, 2, 2, 2, 2, 2, 2, 2, 2, 2, 2, 2, 2, 2, 2, 2, 2, 2, 2, 2, 4 ),
 ( 3, 3 ),
 ( 1.561251128379126385E-17, 0.0008753252358572001296, 0.001312987853785792334, 0.001750650471714384647, 0.002625975707571569055, 0.003501300943428753681, 0.004376626179285938306, 0.004814288797214530402, 0.005251951415143122498, 0.005689614033071714594, 0.006127276651000306690, 0.007002601886857491749, 0.007440264504786084712, 0.007877927122714676808, 0.008315589740643268904, 0.008753252358571861000, 0.009628577594429045192, 0.01050390283028622938, 0.01137922806614341531, 0.01225455330200059950, 0.01269221591992919160, 0.01312987853785778369, 0.01400520377371496789 ),
 ( 0.000000000000000000, 1.000000000000000000 ),
 .UNSPECIFIED. ) 
 GEOMETRIC_REPRESENTATION_ITEM ( )  RATIONAL_B_SPLINE_SURFACE ( (
 ( 1.000000000000000000, 0.7214151048184059833, 1.000000000000000000),
 ( 1.000000000000000000, 0.7139268977831511043, 1.000000000000000000),
 ( 1.000000000000000000, 0.7060919310600005661, 1.000000000000000000),
 ( 1.000000000000000000, 0.6937785501687134815, 1.000000000000000000),
 ( 1.000000000000000000, 0.6895805778049280965, 1.000000000000000000),
 ( 1.000000000000000000, 0.6809903301727727731, 1.000000000000000000),
 ( 1.000000000000000000, 0.6765849663043156381, 1.000000000000000000),
 ( 1.000000000000000000, 0.6633648450980306199, 1.000000000000000000),
 ( 1.000000000000000000, 0.6544550762639834707, 1.000000000000000000),
 ( 1.000000000000000000, 0.6365533617521316190, 1.000000000000000000),
 ( 1.000000000000000000, 0.6275095611399463813, 1.000000000000000000),
 ( 1.000000000000000000, 0.6103974523277966302, 1.000000000000000000),
 ( 1.000000000000000000, 0.6022255868237532672, 1.000000000000000000),
 ( 1.000000000000000000, 0.5908555208068133613, 1.000000000000000000),
 ( 1.000000000000000000, 0.5872289930507547107, 1.000000000000000000),
 ( 1.000000000000000000, 0.5805233329111295637, 1.000000000000000000),
 ( 1.000000000000000000, 0.5774191828807228033, 1.000000000000000000),
 ( 1.000000000000000000, 0.5717609404363922510, 1.000000000000000000),
 ( 1.000000000000000000, 0.5692067459845615573, 1.000000000000000000),
 ( 1.000000000000000000, 0.5647184317875526549, 1.000000000000000000),
 ( 1.000000000000000000, 0.5627791062741893668, 1.000000000000000000),
 ( 1.000000000000000000, 0.5581324696273656238, 1.000000000000000000),
 ( 1.000000000000000000, 0.5565289020892307814, 1.000000000000000000),
 ( 1.000000000000000000, 0.5564933751953636820, 1.000000000000000000),
 ( 1.000000000000000000, 0.5568862388217724613, 1.000000000000000000),
 ( 1.000000000000000000, 0.5584481643512820837, 1.000000000000000000),
 ( 1.000000000000000000, 0.5596129212104073991, 1.000000000000000000),
 ( 1.000000000000000000, 0.5626655503097565125, 1.000000000000000000),
 ( 1.000000000000000000, 0.5645534494397981273, 1.000000000000000000),
 ( 1.000000000000000000, 0.5690213772211072385, 1.000000000000000000),
 ( 1.000000000000000000, 0.5716084335653097703, 1.000000000000000000),
 ( 1.000000000000000000, 0.5801336838986037581, 1.000000000000000000),
 ( 1.000000000000000000, 0.5868791499827269442, 1.000000000000000000),
 ( 1.000000000000000000, 0.6020378157228721827, 1.000000000000000000),
 ( 1.000000000000000000, 0.6103019064041214081, 1.000000000000000000),
 ( 1.000000000000000000, 0.6274511639639016591, 1.000000000000000000),
 ( 1.000000000000000000, 0.6364857471627143326, 1.000000000000000000),
 ( 1.000000000000000000, 0.6544235474393820251, 1.000000000000000000),
 ( 1.000000000000000000, 0.6633507613998016472, 1.000000000000000000),
 ( 1.000000000000000000, 0.6765956464743652088, 1.000000000000000000),
 ( 1.000000000000000000, 0.6810032293232968215, 1.000000000000000000),
 ( 1.000000000000000000, 0.6895857131701266240, 1.000000000000000000),
 ( 1.000000000000000000, 0.6937808971552223980, 1.000000000000000000),
 ( 1.000000000000000000, 0.7060887547132419506, 1.000000000000000000),
 ( 1.000000000000000000, 0.7139238139413449646, 1.000000000000000000),
 ( 1.000000000000000000, 0.7214151048184016535, 1.000000000000000000) ) ) 
 REPRESENTATION_ITEM ( '' )  SURFACE ( )  );
#565 = CARTESIAN_POINT ( 'NONE',  ( -0.05114323250695503725, 0.05905511811023622659, -0.08858267716535432601 ) ) ;
#566 = CARTESIAN_POINT ( 'NONE',  ( 0.05114323250695499562, 0.05905511811023622659, -0.08858267716535433989 ) ) ;
#567 = CARTESIAN_POINT ( 'NONE',  ( -2.011752225599860111, -2.517072610070153260, 0.1485602497173309500 ) ) ;
#568 = CARTESIAN_POINT ( 'NONE',  ( 0.7052242655755273093, -1.858423098537180129, 0.08366141732283417787 ) ) ;
#569 = APPLICATION_PROTOCOL_DEFINITION ( 'draft international standard', 'automotive_design', 1998, #14004 ) ;
#570 = DIRECTION ( 'NONE',  ( 1.349229370204184172E-15, 1.000000000000000000, 0.000000000000000000 ) ) ;
#571 = TOROIDAL_SURFACE ( 'NONE', #3323, 0.5826771653543306728, 0.007874015748031495954 ) ;
#572 = DIRECTION ( 'NONE',  ( -0.000000000000000000, 1.000000000000000000, -0.000000000000000000 ) ) ;
#573 = DIRECTION ( 'NONE',  ( 0.000000000000000000, 1.000000000000000000, -2.602085213965215375E-14 ) ) ;
#574 = CIRCLE ( 'NONE', #3077, 0.05905511811023620578 ) ;
#575 = CARTESIAN_POINT ( 'NONE',  ( 0.000000000000000000, 0.3543307086614172485, 0.000000000000000000 ) ) ;
#576 = CARTESIAN_POINT ( 'NONE',  ( -0.1629063847838169987, -0.4881889763779528324, 0.2122517380126066888 ) ) ;
#577 = DIRECTION ( 'NONE',  ( 0.8660254037844388186, -0.000000000000000000, -0.4999999999999995559 ) ) ;
#578 = ORIENTED_EDGE ( 'NONE', *, *, #12657, .F. ) ;
#579 = VERTEX_POINT ( 'NONE', #4664 ) ;
#580 = EDGE_CURVE ( 'NONE', #7744, #8756, #1058, .T. ) ;
#581 = CARTESIAN_POINT ( 'NONE',  ( -0.1023622047242991467, -0.4881889763779528324, -0.5909884645248154600 ) ) ;
#583 = ORIENTED_EDGE ( 'NONE', *, *, #550, .F. ) ;
#582 = CIRCLE ( 'NONE', #1333, 0.6614173228346456046 ) ;
#584 = AXIS2_PLACEMENT_3D ( 'NONE', #13762, #12668, #13585 ) ;
#585 = ADVANCED_FACE ( 'NONE', ( #5738 ), #15401, .T. ) ;
#586 = ORIENTED_EDGE ( 'NONE', *, *, #12186, .T. ) ;
#587 = CIRCLE ( 'NONE', #2578, 0.003937007874015724558 ) ;
#588 = AXIS2_PLACEMENT_3D ( 'NONE', #13779, #10019, #3044 ) ;
#589 = ADVANCED_FACE ( 'NONE', ( #15242 ), #990, .T. ) ;
#590 = CARTESIAN_POINT ( 'NONE',  ( 0.1724006475077544120, -0.4921259842519685179, 0.1768186671464649640 ) ) ;
#591 = CARTESIAN_POINT ( 'NONE',  ( -1.989672796122207599, -2.818351438590611213, 0.1526128802498082915 ) ) ;
#592 = CARTESIAN_POINT ( 'NONE',  ( -0.6864776960422505070, 1.190944881889763884, 0.4645290592786119332 ) ) ;
#593 =( REPRESENTATION_RELATIONSHIP ('NONE','NONE', #8904, #2403 ) REPRESENTATION_RELATIONSHIP_WITH_TRANSFORMATION ( #2049 )SHAPE_REPRESENTATION_RELATIONSHIP( ) );
#594 = FACE_BOUND ( 'NONE', #5065, .T. ) ;
#595 = DIRECTION ( 'NONE',  ( -0.000000000000000000, -1.000000000000000000, -0.000000000000000000 ) ) ;
#596 = AXIS2_PLACEMENT_3D ( 'NONE', #15015, #4033, #9052 ) ;
#597 = AXIS2_PLACEMENT_3D ( 'NONE', #5978, #13115, #6042 ) ;
#598 = LINE ( 'NONE', #8911, #2398 ) ;
#599 = CARTESIAN_POINT ( 'NONE',  ( -0.3117681530218310848, -0.2952755905511811330, 0.2981971199768678193 ) ) ;
#600 = AXIS2_PLACEMENT_3D ( 'NONE', #3840, #12245, #2907 ) ;
#601 = DIRECTION ( 'NONE',  ( 0.000000000000000000, 0.000000000000000000, 1.000000000000000000 ) ) ;
#602 = CARTESIAN_POINT ( 'NONE',  ( -2.110117761716791218, -1.869184722427368772, -0.1064922012049425715 ) ) ;
#603 = AXIS2_PLACEMENT_3D ( 'NONE', #3145, #649, #11524 ) ;
#604 = ORIENTED_EDGE ( 'NONE', *, *, #2251, .F. ) ;
#605 = ORIENTED_EDGE ( 'NONE', *, *, #7108, .T. ) ;
#606 = ADVANCED_FACE ( 'NONE', ( #11874 ), #11962, .T. ) ;
#607 = ORIENTED_EDGE ( 'NONE', *, *, #5187, .F. ) ;
#608 = ADVANCED_FACE ( 'NONE', ( #9364 ), #6879, .T. ) ;
#609 = EDGE_LOOP ( 'NONE', ( #11562, #301, #9130, #13793 ) ) ;
#610 = ORIENTED_EDGE ( 'NONE', *, *, #10612, .T. ) ;
#611 = VECTOR ( 'NONE', #11502, 39.37007874015748143 ) ;
#612 = VECTOR ( 'NONE', #5962, 39.37007874015748143 ) ;
#613 = LINE ( 'NONE', #2653, #3638 ) ;
#614 = EDGE_CURVE ( 'NONE', #4318, #2230, #12153, .T. ) ;
#615 = CARTESIAN_POINT ( 'NONE',  ( 0.000000000000000000, 0.03149606299212599769, 0.000000000000000000 ) ) ;
#616 = AXIS2_PLACEMENT_3D ( 'NONE', #15267, #1085, #10414 ) ;
#617 = CARTESIAN_POINT ( 'NONE',  ( 0.000000000000000000, 0.05905511811023623353, 0.04527559055118110520 ) ) ;
#618 = CIRCLE ( 'NONE', #13114, 0.003937007874015724558 ) ;
#619 = AXIS2_PLACEMENT_3D ( 'NONE', #2613, #3792, #1368 ) ;
#620 = DIRECTION ( 'NONE',  ( 0.000000000000000000, 0.000000000000000000, -1.000000000000000000 ) ) ;
#621 = DIRECTION ( 'NONE',  ( -4.336808689942015843E-14, 0.000000000000000000, 1.000000000000000000 ) ) ;
#622 = DIRECTION ( 'NONE',  ( 0.000000000000000000, 4.625929269271485914E-16, 1.000000000000000000 ) ) ;
#623 = CARTESIAN_POINT ( 'NONE',  ( -1.942129868064559339, -2.755778082694033682, -0.1769297588256847076 ) ) ;
#624 = VERTEX_POINT ( 'NONE', #8197 ) ;
#625 = FACE_OUTER_BOUND ( 'NONE', #8536, .T. ) ;
#626 = DIRECTION ( 'NONE',  ( 0.5000000000000035527, 0.000000000000000000, -0.8660254037844365982 ) ) ;
#627 = AXIS2_PLACEMENT_3D ( 'NONE', #193, #13095, #1435 ) ;
#628 = VECTOR ( 'NONE', #11097, 39.37007874015748854 ) ;
#629 = CIRCLE ( 'NONE', #15392, 0.04330708661417331101 ) ;
#630 = CLOSED_SHELL ( 'NONE', ( #2826, #6462, #11219, #7557, #8656, #6333, #11542, #4063, #2496, #479, #2527, #9426, #8002, #10340, #3553, #6967, #11921, #6795, #12781, #8537, #1463, #14636, #10299, #12107, #1955, #8483, #10469, #12014, #3014, #10797, #6410, #14699, #14590, #6732, #3320, #12442, #14003, #12202, #11073, #4226, #4468, #3024, #12714, #323, #5299, #9071, #15352, #14777, #10707, #10079, #2785, #13450, #255, #1758, #5659, #12783, #804, #14280, #240, #4507, #7067, #7800, #1378, #3486, #15166, #13336, #7438, #10402, #5977, #4755, #6226, #6125, #9312, #6311, #14243, #11262, #13908, #4731, #14706, #2149, #8957, #7135, #9243, #2881, #1285, #782, #13569, #13309, #6620, #4328, #9213, #5137, #11306, #11414, #10561, #12145, #6624, #3998, #9656, #10949, #9814, #13645, #12298, #7765, #4804, #7297, #8589, #2790, #14496, #7979, #5078, #14559, #6034, #11241, #3602, #3215, #2808, #15273, #3107, #13527, #9923, #1600, #3771, #10508, #3081 ) ) ;
#631 = VERTEX_POINT ( 'NONE', #2299 ) ;
#632 = ORIENTED_EDGE ( 'NONE', *, *, #4758, .T. ) ;
#633 = VECTOR ( 'NONE', #6325, 39.37007874015748143 ) ;
#634 = EDGE_CURVE ( 'NONE', #12118, #2668, #1496, .T. ) ;
#635 = ORIENTED_EDGE ( 'NONE', *, *, #5996, .T. ) ;
#636 = EDGE_CURVE ( 'NONE', #381, #12883, #3392, .T. ) ;
#637 = AXIS2_PLACEMENT_3D ( 'NONE', #3207, #12688, #7976 ) ;
#638 = VECTOR ( 'NONE', #1019, 39.37007874015748143 ) ;
#639 = CIRCLE ( 'NONE', #8141, 0.7007874015748031260 ) ;
#640 = DIRECTION ( 'NONE',  ( -0.8660254037844383745, 0.000000000000000000, -0.5000000000000004441 ) ) ;
#641 = CARTESIAN_POINT ( 'NONE',  ( -0.4854723491485721798, 1.043263280880422528, 0.3484785681409913738 ) ) ;
#642 = DIRECTION ( 'NONE',  ( -0.4999999999999979461, 0.000000000000000000, -0.8660254037844398178 ) ) ;
#643 = DIRECTION ( 'NONE',  ( 0.000000000000000000, -1.000000000000000000, 2.224004456380530778E-16 ) ) ;
#644 = CIRCLE ( 'NONE', #13900, 0.5590551181102362266 ) ;
#645 = DIRECTION ( 'NONE',  ( -0.5000000000000145439, -0.000000000000000000, -0.8660254037844303809 ) ) ;
#646 = VERTEX_POINT ( 'NONE', #6349 ) ;
#647 = CARTESIAN_POINT ( 'NONE',  ( -0.1057717535580962598, -0.1023622047244094474, -0.2491754406047808068 ) ) ;
#648 = ADVANCED_FACE ( 'NONE', ( #12030, #4884 ), #9908, .F. ) ;
#649 = DIRECTION ( 'NONE',  ( 0.000000000000000000, 1.000000000000000000, 0.000000000000000000 ) ) ;
#650 = DIRECTION ( 'NONE',  ( -1.000000000000000000, -0.000000000000000000, -3.476578583725179813E-16 ) ) ;
#651 = CARTESIAN_POINT ( 'NONE',  ( -1.182292270647294030, 0.3416831661896216898, 0.04963306832873103785 ) ) ;
#652 = CARTESIAN_POINT ( 'NONE',  ( 0.000000000000000000, -0.4921259842519685179, 0.000000000000000000 ) ) ;
#653 = AXIS2_PLACEMENT_3D ( 'NONE', #565, #6348, #429 ) ;
#654 = AXIS2_PLACEMENT_3D ( 'NONE', #11086, #7331, #1541 ) ;
#655 = VECTOR ( 'NONE', #5792, 39.37007874015748143 ) ;
#656 = ORIENTED_EDGE ( 'NONE', *, *, #11224, .F. ) ;
#657 = ORIENTED_EDGE ( 'NONE', *, *, #8641, .T. ) ;
#658 = AXIS2_PLACEMENT_3D ( 'NONE', #5672, #10617, #7081 ) ;
#659 = CARTESIAN_POINT ( 'NONE',  ( -0.2681506793016945611, -0.09842519685039370636, 0.03207310886158502850 ) ) ;
#660 = PLANE ( 'NONE',  #160 ) ;
#661 = CARTESIAN_POINT ( 'NONE',  ( -0.04047196874988819026, 0.1700209211169182444, -0.02286660095797711165 ) ) ;
#662 = DIRECTION ( 'NONE',  ( -0.000000000000000000, 1.000000000000000000, -0.000000000000000000 ) ) ;
#663 = PRODUCT_CONTEXT ( 'NONE', #9718, 'mechanical' ) ;
#664 = CIRCLE ( 'NONE', #5395, 2.814960629921260171 ) ;
#665 = CARTESIAN_POINT ( 'NONE',  ( 0.05175539059627461136, 0.06736074103232447818, -0.07475334604056278753 ) ) ;
#666 = CIRCLE ( 'NONE', #1915, 0.03937007874015751446 ) ;
#667 = DIRECTION ( 'NONE',  ( 0.5000000000000041078, -0.000000000000000000, 0.8660254037844363761 ) ) ;
#668 = ORIENTED_EDGE ( 'NONE', *, *, #8195, .F. ) ;
#669 = DIRECTION ( 'NONE',  ( -1.000000000000000000, 0.000000000000000000, 0.000000000000000000 ) ) ;
#670 = ADVANCED_FACE ( 'NONE', ( #1450 ), #9682, .T. ) ;
#671 = DIRECTION ( 'NONE',  ( -0.8660254037844405950, 0.000000000000000000, -0.4999999999999967248 ) ) ;
#672 = DIRECTION ( 'NONE',  ( -0.000000000000000000, -1.000000000000000000, -0.000000000000000000 ) ) ;
#673 = CIRCLE ( 'NONE', #9428, 0.5433070866141731514 ) ;
#674 = CARTESIAN_POINT ( 'NONE',  ( -0.1724006475077544398, -0.4881889763779528324, 0.1728816592724491952 ) ) ;
#675 = VERTEX_POINT ( 'NONE', #14596 ) ;
#676 = ORIENTED_EDGE ( 'NONE', *, *, #10676, .F. ) ;
#677 = VERTEX_POINT ( 'NONE', #1517 ) ;
#678 = AXIS2_PLACEMENT_3D ( 'NONE', #14612, #7540, #13279 ) ;
#679 = ORIENTED_EDGE ( 'NONE', *, *, #14572, .F. ) ;
#680 = AXIS2_PLACEMENT_3D ( 'NONE', #10803, #14428, #249 ) ;
#681 = CARTESIAN_POINT ( 'NONE',  ( -1.509677571405407148, 0.2301488344313167012, -0.03937007874015747977 ) ) ;
#682 = CARTESIAN_POINT ( 'NONE',  ( -1.991652262238867044, -2.812949666188107489, 0.1538927778953757264 ) ) ;
#683 = DIRECTION ( 'NONE',  ( 0.000000000000000000, 0.000000000000000000, 1.000000000000000000 ) ) ;
#684 = AXIS2_PLACEMENT_3D ( 'NONE', #10604, #15073, #15394 ) ;
#685 = DIRECTION ( 'NONE',  ( -0.5692328345973367565, 0.000000000000000000, 0.8221763679505029732 ) ) ;
#686 = DIRECTION ( 'NONE',  ( 0.000000000000000000, 1.000000000000000000, -0.000000000000000000 ) ) ;
#687 = CARTESIAN_POINT ( 'NONE',  ( -0.1872249459500325841, -0.09842519685039370636, -0.1080943729432645994 ) ) ;
#688 = CIRCLE ( 'NONE', #9938, 0.01968503937007873988 ) ;
#689 = DIRECTION ( 'NONE',  ( -0.000000000000000000, -1.000000000000000000, -0.000000000000000000 ) ) ;
#690 = CARTESIAN_POINT ( 'NONE',  ( -2.163017314575554462, -1.630597114118274238, -0.1033464566929129386 ) ) ;
#691 = DIRECTION ( 'NONE',  ( 0.000000000000000000, 0.000000000000000000, -1.000000000000000000 ) ) ;
#692 = VERTEX_POINT ( 'NONE', #1587 ) ;
#693 = EDGE_CURVE ( 'NONE', #3049, #677, #1886, .T. ) ;
#694 = ORIENTED_EDGE ( 'NONE', *, *, #10855, .T. ) ;
#695 = AXIS2_PLACEMENT_3D ( 'NONE', #14577, #5477, #1890 ) ;
#696 = ORIENTED_EDGE ( 'NONE', *, *, #4848, .T. ) ;
#697 = VERTEX_POINT ( 'NONE', #13496 ) ;
#698 = TOROIDAL_SURFACE ( 'NONE', #4699, 0.7007874015748031260, 0.007874015748031495954 ) ;
#699 = CARTESIAN_POINT ( 'NONE',  ( 0.02590706759391969358, 0.06931031770563803041, 0.08113392229587690352 ) ) ;
#700 = FACE_OUTER_BOUND ( 'NONE', #4412, .T. ) ;
#701 = CIRCLE ( 'NONE', #9210, 0.003937007874015758385 ) ;
#702 = EDGE_CURVE ( 'NONE', #15270, #10400, #1155, .T. ) ;
#703 = DIRECTION ( 'NONE',  ( 0.000000000000000000, 0.000000000000000000, 1.000000000000000000 ) ) ;
#704 = CARTESIAN_POINT ( 'NONE',  ( 0.4478092776764652783, 1.043307086614173373, 0.3267337836880532809 ) ) ;
#705 = DIRECTION ( 'NONE',  ( 2.168404344971012655E-14, 0.000000000000000000, 1.000000000000000000 ) ) ;
#706 = DIRECTION ( 'NONE',  ( 1.000000000000000000, 0.000000000000000000, 0.000000000000000000 ) ) ;
#707 = CARTESIAN_POINT ( 'NONE',  ( -1.100415514366370084, -0.04998955061625977997, -0.03937007874015747977 ) ) ;
#708 = EDGE_CURVE ( 'NONE', #13984, #15156, #5125, .T. ) ;
#709 = ORIENTED_EDGE ( 'NONE', *, *, #8054, .F. ) ;
#710 = FACE_OUTER_BOUND ( 'NONE', #1482, .T. ) ;
#711 = DIRECTION ( 'NONE',  ( 0.4999999999999991118, -0.000000000000000000, -0.8660254037844390407 ) ) ;
#712 = AXIS2_PLACEMENT_3D ( 'NONE', #4868, #15319, #10812 ) ;
#713 = VERTEX_POINT ( 'NONE', #14689 ) ;
#714 = EDGE_CURVE ( 'NONE', #4318, #14414, #118, .T. ) ;
#715 = VERTEX_POINT ( 'NONE', #6041 ) ;
#716 = AXIS2_PLACEMENT_3D ( 'NONE', #1330, #14567, #13245 ) ;
#717 = ORIENTED_EDGE ( 'NONE', *, *, #9997, .F. ) ;
#718 = DIRECTION ( 'NONE',  ( 0.000000000000000000, -1.000000000000000000, 0.000000000000000000 ) ) ;
#719 = AXIS2_PLACEMENT_3D ( 'NONE', #11281, #5307, #9175 ) ;
#720 = EDGE_CURVE ( 'NONE', #6036, #11956, #9160, .T. ) ;
#721 = CARTESIAN_POINT ( 'NONE',  ( 0.000000000000000000, 0.000000000000000000, 0.000000000000000000 ) ) ;
#722 = CARTESIAN_POINT ( 'NONE',  ( -0.09842519685028335019, -0.2952755905511811330, -0.4190977005962941981 ) ) ;
#723 = CARTESIAN_POINT ( 'NONE',  ( -1.276200637803905691, -0.1988000726501942539, -0.1033464566929132716 ) ) ;
#724 = CARTESIAN_POINT ( 'NONE',  ( -0.4861941749621833675, 1.338582677165354395, 0.3488953144687877983 ) ) ;
#725 = ADVANCED_FACE ( 'NONE', ( #10826 ), #7386, .F. ) ;
#726 = ORIENTED_EDGE ( 'NONE', *, *, #5696, .T. ) ;
#727 = LINE ( 'NONE', #4011, #1925 ) ;
#728 = CARTESIAN_POINT ( 'NONE',  ( -0.4861941749621833675, 1.338582677165354395, 0.3488953144687877983 ) ) ;
#729 = DIRECTION ( 'NONE',  ( 1.000000000000000000, 1.734723475976817507E-14, 0.000000000000000000 ) ) ;
#730 = CARTESIAN_POINT ( 'NONE',  ( 0.000000000000000000, 0.000000000000000000, -0.5905511811023621549 ) ) ;
#731 = VERTEX_POINT ( 'NONE', #3864 ) ;
#732 = ADVANCED_FACE ( 'NONE', ( #5026 ), #4962, .T. ) ;
#733 = SURFACE_STYLE_FILL_AREA ( #7528 ) ;
#734 = EDGE_LOOP ( 'NONE', ( #10955, #1406, #10244, #12393 ) ) ;
#735 = ORIENTED_EDGE ( 'NONE', *, *, #5267, .F. ) ;
#736 = ORIENTED_EDGE ( 'NONE', *, *, #5648, .T. ) ;
#737 = DIRECTION ( 'NONE',  ( 0.5000000000000001110, 0.000000000000000000, -0.8660254037844385966 ) ) ;
#738 = CYLINDRICAL_SURFACE ( 'NONE', #6887, 0.003937007874015758385 ) ;
#739 = CARTESIAN_POINT ( 'NONE',  ( -0.004432333661848699216, 0.1530140478773363566, -0.007791225829895984979 ) ) ;
#740 = CARTESIAN_POINT ( 'NONE',  ( -0.4788739157331333707, -0.1023622047244094474, 0.3446689608323532661 ) ) ;
#741 = DIRECTION ( 'NONE',  ( 1.000000000000000000, 0.000000000000000000, 0.000000000000000000 ) ) ;
#742 = DIRECTION ( 'NONE',  ( -0.8660254037844385966, 0.000000000000000000, -0.5000000000000001110 ) ) ;
#743 = ORIENTED_EDGE ( 'NONE', *, *, #7868, .F. ) ;
#744 = DIRECTION ( 'NONE',  ( -0.6722799013647171584, 0.7402970580929294497, 0.000000000000000000 ) ) ;
#745 = DIRECTION ( 'NONE',  ( -0.000000000000000000, -1.000000000000000000, -0.000000000000000000 ) ) ;
#746 = CARTESIAN_POINT ( 'NONE',  ( 0.5860051159906326523, -0.09448818897637796532, 0.1591122789105293700 ) ) ;
#747 = EDGE_CURVE ( 'NONE', #3536, #9448, #3643, .T. ) ;
#748 = VERTEX_POINT ( 'NONE', #14368 ) ;
#749 = VERTEX_POINT ( 'NONE', #7305 ) ;
#750 = EDGE_CURVE ( 'NONE', #1302, #7482, #12094, .T. ) ;
#751 = ORIENTED_EDGE ( 'NONE', *, *, #6123, .T. ) ;
#752 = EDGE_CURVE ( 'NONE', #6519, #4716, #5141, .T. ) ;
#753 = DIRECTION ( 'NONE',  ( 0.000000000000000000, 0.000000000000000000, -1.000000000000000000 ) ) ;
#754 = CARTESIAN_POINT ( 'NONE',  ( -2.090051324975687130, -2.010834692585359296, -0.09065852675045296682 ) ) ;
#755 = CARTESIAN_POINT ( 'NONE',  ( 0.03886060139087953863, 0.07874015748031495954, 0.08219815605943972536 ) ) ;
#756 = CARTESIAN_POINT ( 'NONE',  ( 0.4591888763630541104, -0.4881889763779528324, 0.3787644491703230365 ) ) ;
#757 = CARTESIAN_POINT ( 'NONE',  ( -0.07874015748031501505, 0.1442356988431298948, -0.05905511811023622659 ) ) ;
#758 = CARTESIAN_POINT ( 'NONE',  ( 0.4841913566216283216, 1.043107366814280734, 0.3477389867607208473 ) ) ;
#759 = FACE_BOUND ( 'NONE', #6247, .T. ) ;
#760 = EDGE_LOOP ( 'NONE', ( #2647, #10099, #14539, #11090 ) ) ;
#761 = ORIENTED_EDGE ( 'NONE', *, *, #10931, .F. ) ;
#762 = ORIENTED_EDGE ( 'NONE', *, *, #15301, .F. ) ;
#763 = EDGE_LOOP ( 'NONE', ( #10546, #5020, #7300, #14173 ) ) ;
#764 = DIRECTION ( 'NONE',  ( 0.000000000000000000, 0.000000000000000000, -1.000000000000000000 ) ) ;
#765 = DIRECTION ( 'NONE',  ( -0.000000000000000000, 1.000000000000000000, -0.000000000000000000 ) ) ;
#766 = CARTESIAN_POINT ( 'NONE',  ( -2.163017314575554462, -1.630597114118274238, 0.1033464566929129663 ) ) ;
#767 = CARTESIAN_POINT ( 'NONE',  ( 0.2353927734920605308, -0.1023622047244094474, 0.06771310446505662828 ) ) ;
#768 = FACE_OUTER_BOUND ( 'NONE', #1689, .T. ) ;
#769 = CARTESIAN_POINT ( 'NONE',  ( 0.000000000000000000, 1.035433070866142113, 0.000000000000000000 ) ) ;
#770 = DIRECTION ( 'NONE',  ( -0.000000000000000000, -0.000000000000000000, -1.000000000000000000 ) ) ;
#771 = EDGE_LOOP ( 'NONE', ( #6516, #12506, #1056, #668 ) ) ;
#772 = CARTESIAN_POINT ( 'NONE',  ( -0.7796283024904574477, 1.190944881889763884, 0.3819276336347811607 ) ) ;
#773 = DIRECTION ( 'NONE',  ( 0.000000000000000000, 0.000000000000000000, -1.000000000000000000 ) ) ;
#774 = CARTESIAN_POINT ( 'NONE',  ( -0.06692913385815757454, -0.4881889763779528324, -2.418823744386252084E-17 ) ) ;
#775 = PRODUCT_DEFINITION_SHAPE ( 'NONE', 'NONE',  #3339 ) ;
#776 = VERTEX_POINT ( 'NONE', #10995 ) ;
#777 = VERTEX_POINT ( 'NONE', #9823 ) ;
#778 = EDGE_CURVE ( 'NONE', #7384, #11994, #8647, .T. ) ;
#779 = ORIENTED_EDGE ( 'NONE', *, *, #7891, .F. ) ;
#780 = EDGE_CURVE ( 'NONE', #25, #15217, #5492, .T. ) ;
#781 = CARTESIAN_POINT ( 'NONE',  ( -1.509677571405407148, 0.2301488344313167012, 0.05905511811023622659 ) ) ;
#782 = ADVANCED_FACE ( 'NONE', ( #12408, #13806 ), #660, .T. ) ;
#783 = CARTESIAN_POINT ( 'NONE',  ( 0.000000000000000000, 2.393700787401575436, 0.000000000000000000 ) ) ;
#784 = DIRECTION ( 'NONE',  ( 0.000000000000000000, 0.000000000000000000, 1.000000000000000000 ) ) ;
#785 = DIRECTION ( 'NONE',  ( -0.000000000000000000, 1.000000000000000000, -0.000000000000000000 ) ) ;
#786 = CARTESIAN_POINT ( 'NONE',  ( 0.1586168312385622392, -0.09842519685039370636, -0.5890199605878065903 ) ) ;
#787 = ORIENTED_EDGE ( 'NONE', *, *, #7677, .F. ) ;
#788 = DIRECTION ( 'NONE',  ( -0.5000000000000004441, -0.000000000000000000, -0.8660254037844384856 ) ) ;
#789 = DIRECTION ( 'NONE',  ( 0.000000000000000000, 0.000000000000000000, -1.000000000000000000 ) ) ;
#790 = FACE_OUTER_BOUND ( 'NONE', #8805, .T. ) ;
#791 = LINE ( 'NONE', #6898, #14091 ) ;
#792 = ORIENTED_EDGE ( 'NONE', *, *, #77, .F. ) ;
#793 = CYLINDRICAL_SURFACE ( 'NONE', #11958, 0.003937007874015750579 ) ;
#794 = ORIENTED_EDGE ( 'NONE', *, *, #9584, .F. ) ;
#795 = EDGE_CURVE ( 'NONE', #13551, #646, #5417, .T. ) ;
#796 = VERTEX_POINT ( 'NONE', #12639 ) ;
#797 = EDGE_CURVE ( 'NONE', #9540, #1289, #4399, .T. ) ;
#798 = ORIENTED_EDGE ( 'NONE', *, *, #7205, .T. ) ;
#799 = DIRECTION ( 'NONE',  ( 0.000000000000000000, -1.000000000000000000, -0.000000000000000000 ) ) ;
#800 = CARTESIAN_POINT ( 'NONE',  ( 9.360245101547351149E-18, 0.07093549527207514138, 0.07900545476875124595 ) ) ;
#801 = ADVANCED_FACE ( 'NONE', ( #8881 ), #738, .T. ) ;
#802 = CARTESIAN_POINT ( 'NONE',  ( 0.7052242655755273093, -1.858423098537180129, 0.1968503937007874127 ) ) ;
#803 = CYLINDRICAL_SURFACE ( 'NONE', #15382, 0.1279527559055117780 ) ;
#804 = ADVANCED_FACE ( 'NONE', ( #11143, #1678 ), #3068, .F. ) ;
#805 = DIRECTION ( 'NONE',  ( -0.5000000000000028866, -0.000000000000000000, 0.8660254037844371533 ) ) ;
#806 = DIRECTION ( 'NONE',  ( 0.4999999999999979461, 0.000000000000000000, 0.8660254037844398178 ) ) ;
#807 = ORIENTED_EDGE ( 'NONE', *, *, #14959, .T. ) ;
#808 = CYLINDRICAL_SURFACE ( 'NONE', #14177, 0.03937007874015754916 ) ;
#809 = DIRECTION ( 'NONE',  ( 0.000000000000000000, -1.000000000000000000, -0.000000000000000000 ) ) ;
#810 = DIRECTION ( 'NONE',  ( 0.8660254037844398178, -0.000000000000000000, -0.4999999999999979461 ) ) ;
#811 = EDGE_LOOP ( 'NONE', ( #1997, #5279, #9049, #3550, #14729 ) ) ;
#812 = ORIENTED_EDGE ( 'NONE', *, *, #2440, .T. ) ;
#813 = DIRECTION ( 'NONE',  ( -0.8660254037844385966, 0.000000000000000000, 0.5000000000000002220 ) ) ;
#814 = ORIENTED_EDGE ( 'NONE', *, *, #8460, .F. ) ;
#815 = ORIENTED_EDGE ( 'NONE', *, *, #7483, .T. ) ;
#816 = LINE ( 'NONE', #8025, #356 ) ;
#817 = CARTESIAN_POINT ( 'NONE',  ( -1.332606523864378945, 0.1355266887446167634, -0.03937007874015747977 ) ) ;
#818 = ADVANCED_FACE ( 'NONE', ( #1749 ), #895, .T. ) ;
#819 = CARTESIAN_POINT ( 'NONE',  ( 0.6864776960422569463, 1.190944881889763884, 0.4645290592786023298 ) ) ;
#820 = DIRECTION ( 'NONE',  ( -0.4999999999999996114, -0.000000000000000000, -0.8660254037844389297 ) ) ;
#821 = CARTESIAN_POINT ( 'NONE',  ( 0.1022864650139100745, 0.05905511811023622659, 1.563012696487738457E-17 ) ) ;
#822 = ADVANCED_FACE ( 'NONE', ( #9035 ), #7844, .F. ) ;
#823 = CARTESIAN_POINT ( 'NONE',  ( 0.000000000000000000, 0.4133858267716535306, -0.03937007874015747977 ) ) ;
#824 = PLANE ( 'NONE',  #13907 ) ;
#825 = VECTOR ( 'NONE', #4213, 39.37007874015748143 ) ;
#826 = AXIS2_PLACEMENT_3D ( 'NONE', #6958, #14170, #7030 ) ;
#827 = ORIENTED_EDGE ( 'NONE', *, *, #13928, .T. ) ;
#828 = CIRCLE ( 'NONE', #11072, 0.7007874015748031260 ) ;
#829 = ORIENTED_EDGE ( 'NONE', *, *, #9644, .F. ) ;
#830 = CIRCLE ( 'NONE', #2083, 0.5826771653543306728 ) ;
#831 = ORIENTED_EDGE ( 'NONE', *, *, #6721, .F. ) ;
#832 = ORIENTED_EDGE ( 'NONE', *, *, #3269, .F. ) ;
#833 = CARTESIAN_POINT ( 'NONE',  ( -0.1062992125983150127, -0.1023622047244094474, -0.2482618547482104143 ) ) ;
#834 = DIRECTION ( 'NONE',  ( 0.000000000000000000, -1.000000000000000000, 0.000000000000000000 ) ) ;
#835 = VECTOR ( 'NONE', #4975, 39.37007874015748143 ) ;
#836 = DIRECTION ( 'NONE',  ( 0.000000000000000000, 0.000000000000000000, 1.000000000000000000 ) ) ;
#837 = AXIS2_PLACEMENT_3D ( 'NONE', #6207, #2532, #7307 ) ;
#838 = CARTESIAN_POINT ( 'NONE',  ( -0.004867930653576267239, 0.1761271985363120074, 0.009096853601420660032 ) ) ;
#839 = VECTOR ( 'NONE', #7017, 39.37007874015748143 ) ;
#840 = DIRECTION ( 'NONE',  ( 0.000000000000000000, 0.000000000000000000, -1.000000000000000000 ) ) ;
#841 = DIRECTION ( 'NONE',  ( 0.8660254037844397068, 0.000000000000000000, -0.4999999999999981681 ) ) ;
#842 = CIRCLE ( 'NONE', #2095, 0.003937007874015758385 ) ;
#843 = DIRECTION ( 'NONE',  ( 1.000000000000000000, 0.000000000000000000, 0.000000000000000000 ) ) ;
#844 = DIRECTION ( 'NONE',  ( -0.000000000000000000, -0.000000000000000000, -1.000000000000000000 ) ) ;
#845 = ORIENTED_EDGE ( 'NONE', *, *, #9115, .F. ) ;
#846 = DIRECTION ( 'NONE',  ( -0.000000000000000000, 1.000000000000000000, 0.000000000000000000 ) ) ;
#847 = ADVANCED_FACE ( 'NONE', ( #10281, #4174 ), #15060, .T. ) ;
#848 = DIRECTION ( 'NONE',  ( -0.8660254037844347108, 0.000000000000000000, -0.5000000000000069944 ) ) ;
#849 = DIRECTION ( 'NONE',  ( -0.000000000000000000, -0.000000000000000000, 1.000000000000000000 ) ) ;
#850 = ORIENTED_EDGE ( 'NONE', *, *, #11015, .F. ) ;
#851 = VERTEX_POINT ( 'NONE', #13886 ) ;
#852 = AXIS2_PLACEMENT_3D ( 'NONE', #6869, #11661, #10090 ) ;
#853 = AXIS2_PLACEMENT_3D ( 'NONE', #1926, #10536, #6764 ) ;
#854 = AXIS2_PLACEMENT_3D ( 'NONE', #12975, #4803, #3424 ) ;
#855 = CIRCLE ( 'NONE', #11365, 0.5905511811023621549 ) ;
#856 = VERTEX_POINT ( 'NONE', #430 ) ;
#857 = CIRCLE ( 'NONE', #5594, 0.003937007874015754916 ) ;
#858 = DIRECTION ( 'NONE',  ( 0.000000000000000000, 0.000000000000000000, -1.000000000000000000 ) ) ;
#859 = AXIS2_PLACEMENT_3D ( 'NONE', #46, #9686, #12262 ) ;
#860 = CARTESIAN_POINT ( 'NONE',  ( 0.1062992125984796032, -0.4921259842519685179, -0.2482618547481154347 ) ) ;
#861 = CARTESIAN_POINT ( 'NONE',  ( -1.925560620047871874, -2.948015126518888529, 0.02361865587082091072 ) ) ;
#862 = DIRECTION ( 'NONE',  ( -0.000000000000000000, -1.000000000000000000, -0.000000000000000000 ) ) ;
#863 = VECTOR ( 'NONE', #13257, 39.37007874015748143 ) ;
#864 = DIRECTION ( 'NONE',  ( 0.000000000000000000, 1.000000000000000000, 0.000000000000000000 ) ) ;
#865 = AXIS2_PLACEMENT_3D ( 'NONE', #7504, #5524, #3341 ) ;
#866 = AXIS2_PLACEMENT_3D ( 'NONE', #3653, #8735, #8428 ) ;
#867 = DIRECTION ( 'NONE',  ( 0.000000000000000000, -0.000000000000000000, -1.000000000000000000 ) ) ;
#868 = ORIENTED_EDGE ( 'NONE', *, *, #1236, .F. ) ;
#869 = CARTESIAN_POINT ( 'NONE',  ( -1.181102362204724310, 0.000000000000000000, -0.02952755905511811330 ) ) ;
#870 = AXIS2_PLACEMENT_3D ( 'NONE', #10796, #14421, #2198 ) ;
#871 = DIRECTION ( 'NONE',  ( 1.000000000000000000, 0.000000000000000000, 0.000000000000000000 ) ) ;
#872 = AXIS2_PLACEMENT_3D ( 'NONE', #13790, #7826, #4231 ) ;
#873 = ADVANCED_FACE ( 'NONE', ( #5181 ), #10899, .T. ) ;
#874 = CARTESIAN_POINT ( 'NONE',  ( -1.419615703680148000, -0.01226548409420232313, -0.08366141732283458032 ) ) ;
#875 = ORIENTED_EDGE ( 'NONE', *, *, #9352, .T. ) ;
#876 = CARTESIAN_POINT ( 'NONE',  ( -1.181102362204724310, 0.000000000000000000, -0.02952755905511811330 ) ) ;
#877 = VERTEX_POINT ( 'NONE', #8967 ) ;
#878 = EDGE_CURVE ( 'NONE', #7659, #6985, #13741, .T. ) ;
#880 = VERTEX_POINT ( 'NONE', #8794 ) ;
#879 = AXIS2_PLACEMENT_3D ( 'NONE', #11902, #67, #11817 ) ;
#881 = CIRCLE ( 'NONE', #8384, 0.007874015748031449116 ) ;
#882 = CARTESIAN_POINT ( 'NONE',  ( -0.2362204724409448231, -0.02638708502139245488, 0.05905511811023622659 ) ) ;
#883 = AXIS2_PLACEMENT_3D ( 'NONE', #6783, #8220, #5691 ) ;
#884 = CARTESIAN_POINT ( 'NONE',  ( -1.591501945092674841, 0.08600752902535288569, -0.08366141732283462196 ) ) ;
#885 = CARTESIAN_POINT ( 'NONE',  ( 0.05905511811029064834, -0.1023622047244094474, -0.5870514566507987197 ) ) ;
#886 = ITEM_DEFINED_TRANSFORMATION ( 'NONE', 'NONE', #5205,  #11481 ) ;
#887 = CARTESIAN_POINT ( 'NONE',  ( 0.4296613173079339432, -0.09448818897637796532, 0.4299076816772811060 ) ) ;
#888 = DIRECTION ( 'NONE',  ( -0.9162674345903500939, 0.4005670834070347297, 0.000000000000000000 ) ) ;
#889 = EDGE_LOOP ( 'NONE', ( #5300, #4624, #9223, #8545, #11790, #12162, #13483 ) ) ;
#890 = FACE_OUTER_BOUND ( 'NONE', #9539, .T. ) ;
#891 = PLANE ( 'NONE',  #2622 ) ;
#892 = AXIS2_PLACEMENT_3D ( 'NONE', #1259, #7211, #9414 ) ;
#893 = CARTESIAN_POINT ( 'NONE',  ( 8.582170482213735190E-17, 0.3228346456692913757, -0.7007874015748031260 ) ) ;
#894 = EDGE_CURVE ( 'NONE', #2999, #13968, #13406, .T. ) ;
#895 = TOROIDAL_SURFACE ( 'NONE', #4145, 0.04330708661417328326, 0.003937007874015747977 ) ;
#896 = SURFACE_STYLE_USAGE ( .BOTH. , #5731 ) ;
#897 = VERTEX_POINT ( 'NONE', #11228 ) ;
#898 = CIRCLE ( 'NONE', #10156, 0.01968503937007875723 ) ;
#899 = ORIENTED_EDGE ( 'NONE', *, *, #2261, .F. ) ;
#900 = APPLICATION_CONTEXT ( 'automotive_design' ) ;
#901 = EDGE_CURVE ( 'NONE', #8071, #4513, #9408, .T. ) ;
#902 = FACE_OUTER_BOUND ( 'NONE', #2102, .T. ) ;
#903 = ORIENTED_EDGE ( 'NONE', *, *, #9642, .T. ) ;
#904 = EDGE_LOOP ( 'NONE', ( #14618, #3065, #11206, #13154, #5873, #3253, #1821, #183, #12999, #7983 ) ) ;
#905 = ORIENTED_EDGE ( 'NONE', *, *, #7727, .F. ) ;
#906 = VECTOR ( 'NONE', #11172, 39.37007874015748143 ) ;
#907 =( GEOMETRIC_REPRESENTATION_CONTEXT ( 3 ) GLOBAL_UNCERTAINTY_ASSIGNED_CONTEXT ( ( #5158 ) ) GLOBAL_UNIT_ASSIGNED_CONTEXT ( ( #9292, #7018, #5913 ) ) REPRESENTATION_CONTEXT ( 'NONE', 'WORKASPACE' ) );
#908 = AXIS2_PLACEMENT_3D ( 'NONE', #8038, #4517, #13842 ) ;
#909 = CYLINDRICAL_SURFACE ( 'NONE', #12864, 0.03937007874015747977 ) ;
#910 = FACE_OUTER_BOUND ( 'NONE', #11631, .T. ) ;
#911 = B_SPLINE_CURVE_WITH_KNOTS ( 'NONE', 3,
 ( #9915, #1684, #1754, #1594 ),
 .UNSPECIFIED., .F., .F.,
 ( 4, 4 ),
 ( 0.01504928987911790389, 0.01565334703627738883 ),
 .UNSPECIFIED. ) ;
#912 =( LENGTH_UNIT ( ) NAMED_UNIT ( * ) SI_UNIT ( $, .METRE. ) );
#913 = CIRCLE ( 'NONE', #12421, 0.003937007874015746242 ) ;
#914 = PRODUCT_DEFINITION_SHAPE ( 'NONE', 'NONE',  #6099 ) ;
#915 = CARTESIAN_POINT ( 'NONE',  ( -1.100415514366356762, -0.04998955061627542718, 0.03937007874015747977 ) ) ;
#916 = ADVANCED_FACE ( 'NONE', ( #13090 ), #10678, .T. ) ;
#917 = CARTESIAN_POINT ( 'NONE',  ( 4.821444091131316146E-18, 0.07480314960629921850, 0.03937007874015751446 ) ) ;
#918 = EDGE_CURVE ( 'NONE', #12092, #8071, #5647, .T. ) ;
#919 = CARTESIAN_POINT ( 'NONE',  ( -1.398495881576244493, -0.02731002314121872693, 0.08366141732283458032 ) ) ;
#920 = DIRECTION ( 'NONE',  ( 0.000000000000000000, -0.000000000000000000, -1.000000000000000000 ) ) ;
#921=STYLED_ITEM('',(#15533),#9543);
#922 = ORIENTED_EDGE ( 'NONE', *, *, #780, .T. ) ;
#923 = EDGE_CURVE ( 'NONE', #8145, #9678, #5626, .T. ) ;
#924 = VERTEX_POINT ( 'NONE', #5720 ) ;
#925 = VERTEX_POINT ( 'NONE', #8076 ) ;
#926 = VECTOR ( 'NONE', #8716, 39.37007874015748143 ) ;
#927 = ORIENTED_EDGE ( 'NONE', *, *, #4510, .F. ) ;
#928 = VECTOR ( 'NONE', #570, 39.37007874015748143 ) ;
#929 = ADVANCED_FACE ( 'NONE', ( #3475 ), #12950, .T. ) ;
#930 = FACE_OUTER_BOUND ( 'NONE', #13768, .T. ) ;
#931 = DIRECTION ( 'NONE',  ( 0.8660254037844361541, 0.000000000000000000, -0.5000000000000042188 ) ) ;
#932 =( GEOMETRIC_REPRESENTATION_CONTEXT ( 3 ) GLOBAL_UNCERTAINTY_ASSIGNED_CONTEXT ( ( #2508 ) ) GLOBAL_UNIT_ASSIGNED_CONTEXT ( ( #2686, #3784, #14587 ) ) REPRESENTATION_CONTEXT ( 'NONE', 'WORKASPACE' ) );
#933 = DIRECTION ( 'NONE',  ( 1.224646799147353207E-16, 1.000000000000000000, -0.000000000000000000 ) ) ;
#934 = DIRECTION ( 'NONE',  ( -1.000000000000000000, 0.000000000000000000, 0.000000000000000000 ) ) ;
#935 = CARTESIAN_POINT ( 'NONE',  ( -0.1574803149606299191, -0.09842519685039370636, -0.5909884645248143498 ) ) ;
#936 = AXIS2_PLACEMENT_3D ( 'NONE', #5152, #9872, #6548 ) ;
#937 = CARTESIAN_POINT ( 'NONE',  ( -1.923247296301440645, -2.877714865856489723, -0.1429548596504897628 ) ) ;
#938 = ORIENTED_EDGE ( 'NONE', *, *, #13456, .F. ) ;
#939 = DIRECTION ( 'NONE',  ( 0.5984233124757303290, 0.8011800915434523773, -4.135314009930608449E-15 ) ) ;
#940 = DIRECTION ( 'NONE',  ( 0.5750876580239419056, 0.8180917953313906477, 0.000000000000000000 ) ) ;
#941 = TOROIDAL_SURFACE ( 'NONE', #3941, 0.03937007874015747977, 0.01968503937007873988 ) ;
#942 = EDGE_LOOP ( 'NONE', ( #5409, #11759, #13942 ) ) ;
#943 = ORIENTED_EDGE ( 'NONE', *, *, #10484, .T. ) ;
#944 = EDGE_CURVE ( 'NONE', #7482, #14862, #6374, .T. ) ;
#945 = AXIS2_PLACEMENT_3D ( 'NONE', #4820, #8441, #8672 ) ;
#946 = ORIENTED_EDGE ( 'NONE', *, *, #3969, .F. ) ;
#947 = MECHANICAL_DESIGN_GEOMETRIC_PRESENTATION_REPRESENTATION (  '', ( #3202 ), #15213 ) ;
#948 = EDGE_CURVE ( 'NONE', #7254, #2901, #10655, .T. ) ;
#949 = DIRECTION ( 'NONE',  ( 0.000000000000000000, 0.000000000000000000, -1.000000000000000000 ) ) ;
#950 = EDGE_CURVE ( 'NONE', #450, #856, #14205, .T. ) ;
#951 = CIRCLE ( 'NONE', #15455, 0.003937007874015749712 ) ;
#952 = DIRECTION ( 'NONE',  ( 0.000000000000000000, -1.000000000000000000, 0.000000000000000000 ) ) ;
#953 = CARTESIAN_POINT ( 'NONE',  ( -1.985311755390326782, -2.772329397582949717, -0.1771653543307079026 ) ) ;
#954 = CARTESIAN_POINT ( 'NONE',  ( -0.1763376553817701531, -0.09842519685039370636, 0.1699995694788710154 ) ) ;
#956 = VECTOR ( 'NONE', #4035, 39.37007874015748143 ) ;
#955 = LINE ( 'NONE', #4538, #13612 ) ;
#957 = DIRECTION ( 'NONE',  ( 0.000000000000000000, 0.000000000000000000, 1.000000000000000000 ) ) ;
#958 = ORIENTED_EDGE ( 'NONE', *, *, #7721, .T. ) ;
#959 = DIRECTION ( 'NONE',  ( -1.000000000000000000, 0.000000000000000000, 0.000000000000000000 ) ) ;
#960 = FACE_OUTER_BOUND ( 'NONE', #1382, .T. ) ;
#961 = AXIS2_PLACEMENT_3D ( 'NONE', #4474, #2274, #12778 ) ;
#962 = CARTESIAN_POINT ( 'NONE',  ( -0.008251140381529234111, 0.1525182358981298780, 0.01646613645217641017 ) ) ;
#963 = CYLINDRICAL_SURFACE ( 'NONE', #11859, 0.003937007874015743640 ) ;
#964 = ORIENTED_EDGE ( 'NONE', *, *, #4575, .F. ) ;
#965 = DIRECTION ( 'NONE',  ( 1.734723475976807094E-14, -1.000000000000000000, 0.000000000000000000 ) ) ;
#966 = ORIENTED_EDGE ( 'NONE', *, *, #12026, .F. ) ;
#967 = ORIENTED_EDGE ( 'NONE', *, *, #948, .F. ) ;
#968 = AXIS2_PLACEMENT_3D ( 'NONE', #11211, #6190, #9746 ) ;
#969 = ORIENTED_EDGE ( 'NONE', *, *, #11355, .T. ) ;
#970 = LINE ( 'NONE', #8966, #14340 ) ;
#971 = DIRECTION ( 'NONE',  ( 0.000000000000000000, 0.000000000000000000, 1.000000000000000000 ) ) ;
#972 = AXIS2_PLACEMENT_3D ( 'NONE', #13362, #5995, #1533 ) ;
#973 = CARTESIAN_POINT ( 'NONE',  ( -0.1552072824047652788, -0.09842519685039370636, -0.5909884645248143498 ) ) ;
#974 = DIRECTION ( 'NONE',  ( -1.000000000000000000, 0.000000000000000000, 0.000000000000000000 ) ) ;
#975 = CONTEXT_DEPENDENT_SHAPE_REPRESENTATION ( #12108, #11674 ) ;
#976 = CARTESIAN_POINT ( 'NONE',  ( -0.5905511811023629321, -0.09842519685039370636, 0.1591122789105256785 ) ) ;
#977 = ORIENTED_EDGE ( 'NONE', *, *, #15068, .F. ) ;
#978 = CARTESIAN_POINT ( 'NONE',  ( -1.941057606383688183, -2.905071431831486528, -0.1180179303142062930 ) ) ;
#979 = DIRECTION ( 'NONE',  ( 1.000000000000000000, 0.000000000000000000, 0.000000000000000000 ) ) ;
#980 = DIRECTION ( 'NONE',  ( 0.000000000000000000, 0.000000000000000000, 1.000000000000000000 ) ) ;
#981 = DIRECTION ( 'NONE',  ( 0.000000000000000000, 0.000000000000000000, -1.000000000000000000 ) ) ;
#982 = FILL_AREA_STYLE_COLOUR ( '', #14679 ) ;
#983 = ORIENTED_EDGE ( 'NONE', *, *, #1673, .T. ) ;
#984 = VERTEX_POINT ( 'NONE', #2046 ) ;
#985 = DIRECTION ( 'NONE',  ( 0.000000000000000000, 0.000000000000000000, 1.000000000000000000 ) ) ;
#986 = VERTEX_POINT ( 'NONE', #6991 ) ;
#987 = ORIENTED_EDGE ( 'NONE', *, *, #4982, .T. ) ;
#988 = EDGE_CURVE ( 'NONE', #8756, #6899, #3902, .T. ) ;
#989 = ORIENTED_EDGE ( 'NONE', *, *, #10688, .F. ) ;
#990 = SPHERICAL_SURFACE ( 'NONE', #13637, 0.003937007874015747977 ) ;
#991 = EDGE_CURVE ( 'NONE', #6292, #13356, #14275, .T. ) ;
#992 = DIRECTION ( 'NONE',  ( 0.000000000000000000, 0.000000000000000000, -1.000000000000000000 ) ) ;
#993 = CARTESIAN_POINT ( 'NONE',  ( -1.897883522938190959, -2.949475805367709480, 0.01220870853311090999 ) ) ;
#994 =( NAMED_UNIT ( * ) PLANE_ANGLE_UNIT ( ) SI_UNIT ( $, .RADIAN. ) );
#995 = DIRECTION ( 'NONE',  ( 0.8660254037844385966, 0.000000000000000000, 0.5000000000000001110 ) ) ;
#996 = CARTESIAN_POINT ( 'NONE',  ( 0.03886060139087953863, 0.000000000000000000, 0.08219815605943972536 ) ) ;
#997 = CARTESIAN_POINT ( 'NONE',  ( -0.1062992125983148878, -0.1023622047244094474, -0.5909884645248154600 ) ) ;
#998 = EDGE_CURVE ( 'NONE', #10209, #986, #14164, .T. ) ;
#999 =( BOUNDED_CURVE ( )  B_SPLINE_CURVE ( 3, ( #2540, #2769, #12110, #13214 ),
 .UNSPECIFIED., .F., .T. ) 
 B_SPLINE_CURVE_WITH_KNOTS ( ( 4, 4 ),
 ( 3.141592653589793116, 4.712388980384689674 ),
 .UNSPECIFIED. ) 
 CURVE ( )  GEOMETRIC_REPRESENTATION_ITEM ( )  RATIONAL_B_SPLINE_CURVE ( ( 1.000000000000000000, 0.8047378541243649375, 0.8047378541243649375, 1.000000000000000000 ) ) 
 REPRESENTATION_ITEM ( '' )  );
#1000 = DIRECTION ( 'NONE',  ( -0.000000000000000000, 0.000000000000000000, 1.000000000000000000 ) ) ;
#1001 = CARTESIAN_POINT ( 'NONE',  ( 0.000000000000000000, 0.4133858267716535306, 0.000000000000000000 ) ) ;
#1002 = CARTESIAN_POINT ( 'NONE',  ( 1.880363195541211833E-17, -0.4881889763779528324, 0.1535433070866141780 ) ) ;
#1003 = DIRECTION ( 'NONE',  ( -1.000000000000000000, 0.000000000000000000, 0.000000000000000000 ) ) ;
#1004 = VERTEX_POINT ( 'NONE', #800 ) ;
#1005 = ORIENTED_EDGE ( 'NONE', *, *, #4307, .F. ) ;
#1006 = EDGE_LOOP ( 'NONE', ( #11275, #9630, #2726, #9101 ) ) ;
#1007 = ORIENTED_EDGE ( 'NONE', *, *, #3290, .F. ) ;
#1008 = EDGE_CURVE ( 'NONE', #9261, #6774, #14410, .T. ) ;
#1009 = DIRECTION ( 'NONE',  ( 0.8660254037844365982, -0.000000000000000000, 0.5000000000000035527 ) ) ;
#1010 = DIRECTION ( 'NONE',  ( 0.000000000000000000, -1.000000000000000000, 0.000000000000000000 ) ) ;
#1011 = CARTESIAN_POINT ( 'NONE',  ( -0.03726199245315515995, 0.1489178558047651590, 0.04781523662142502656 ) ) ;
#1012 = EDGE_CURVE ( 'NONE', #6200, #9631, #5093, .T. ) ;
#1013 = CARTESIAN_POINT ( 'NONE',  ( -0.5403775459648845203, 1.343094183513034778, 0.2394881783597615499 ) ) ;
#1014 = DIRECTION ( 'NONE',  ( 1.000000000000000000, 0.000000000000000000, -1.224646799147353207E-16 ) ) ;
#1015 = DIRECTION ( 'NONE',  ( 1.000000000000000000, 0.000000000000000000, 0.000000000000000000 ) ) ;
#1016 = ORIENTED_EDGE ( 'NONE', *, *, #2937, .T. ) ;
#1017 = CARTESIAN_POINT ( 'NONE',  ( 0.4572203724260462399, -0.4921259842519685179, 0.3821739980041199969 ) ) ;
#1018 = DIRECTION ( 'NONE',  ( -1.224646799147352961E-16, 0.000000000000000000, -1.000000000000000000 ) ) ;
#1019 = DIRECTION ( 'NONE',  ( -0.000000000000000000, -0.000000000000000000, -1.000000000000000000 ) ) ;
#1020 = ORIENTED_EDGE ( 'NONE', *, *, #4376, .F. ) ;
#1021 = ORIENTED_EDGE ( 'NONE', *, *, #276, .F. ) ;
#1022 = EDGE_LOOP ( 'NONE', ( #5341, #2667 ) ) ;
#1023 = DIRECTION ( 'NONE',  ( 0.4999999999999981681, -0.000000000000000000, 0.8660254037844397068 ) ) ;
#1024 = FACE_OUTER_BOUND ( 'NONE', #5897, .T. ) ;
#1025 = CARTESIAN_POINT ( 'NONE',  ( -1.925013044204064050, -2.949504264475041992, 0.005679328437135281946 ) ) ;
#1026 = EDGE_CURVE ( 'NONE', #6685, #10277, #11654, .T. ) ;
#1027 = DIRECTION ( 'NONE',  ( -0.000000000000000000, -0.000000000000000000, -1.000000000000000000 ) ) ;
#1028 = DIRECTION ( 'NONE',  ( 0.5000000000000004441, 3.469446951953638170E-14, 0.8660254037844383745 ) ) ;
#1029 = DIRECTION ( 'NONE',  ( 0.000000000000000000, -1.000000000000000000, 0.000000000000000000 ) ) ;
#1030 = EDGE_LOOP ( 'NONE', ( #7422, #792, #11889, #9381 ) ) ;
#1031 = CARTESIAN_POINT ( 'NONE',  ( 0.5412478373021326616, 1.035433070866141891, 0.2362233606508025163 ) ) ;
#1032 = CARTESIAN_POINT ( 'NONE',  ( -0.06604848736013263499, 0.000000000000000000, -0.5868460571724355423 ) ) ;
#1033 = CARTESIAN_POINT ( 'NONE',  ( -0.06155496847469425076, 0.1461038053415525118, 0.05764730824460247843 ) ) ;
#1034 = DIRECTION ( 'NONE',  ( 0.000000000000000000, 0.000000000000000000, -1.000000000000000000 ) ) ;
#1035 = ORIENTED_EDGE ( 'NONE', *, *, #10958, .T. ) ;
#1036 = ADVANCED_FACE ( 'NONE', ( #15374 ), #11609, .F. ) ;
#1037 = EDGE_LOOP ( 'NONE', ( #270, #7446, #2193, #12989, #1239, #3316, #6250, #4471, #9799, #11494, #534, #1260, #10547, #8192, #10475, #4205 ) ) ;
#1038 = ORIENTED_EDGE ( 'NONE', *, *, #11523, .T. ) ;
#1039 = EDGE_LOOP ( 'NONE', ( #9659, #9479, #4658, #5021 ) ) ;
#1040 = ORIENTED_EDGE ( 'NONE', *, *, #9642, .F. ) ;
#1041 = B_SPLINE_CURVE_WITH_KNOTS ( 'NONE', 3,
 ( #1316, #2555, #10867, #4984 ),
 .UNSPECIFIED., .F., .F.,
 ( 4, 4 ),
 ( 0.000000000000000000, 2.119993237936519055E-05 ),
 .UNSPECIFIED. ) ;
#1042 = DIRECTION ( 'NONE',  ( 0.000000000000000000, 1.000000000000000000, 0.000000000000000000 ) ) ;
#1043 = DIRECTION ( 'NONE',  ( -1.000000000000000000, -0.000000000000000000, -3.476578583725179813E-16 ) ) ;
#1044 = CARTESIAN_POINT ( 'NONE',  ( 1.181102362204724310, 4.044111181948214319E-16, 0.02559055118110236185 ) ) ;
#1045 = CARTESIAN_POINT ( 'NONE',  ( -0.07874015748031494566, 0.1685051786281938357, 0.03937007874015747977 ) ) ;
#1046 = CONTEXT_DEPENDENT_SHAPE_REPRESENTATION ( #593, #5645 ) ;
#1047 = LINE ( 'NONE', #11852, #8451 ) ;
#1048 = DIRECTION ( 'NONE',  ( 1.000000000000000000, 0.000000000000000000, 3.075191616504340279E-15 ) ) ;
#1049 = EDGE_LOOP ( 'NONE', ( #4952, #1462, #9924, #12331 ) ) ;
#1050 = DIRECTION ( 'NONE',  ( -0.000000000000000000, 0.000000000000000000, 1.000000000000000000 ) ) ;
#1051 = LINE ( 'NONE', #12875, #3373 ) ;
#1052 = DIRECTION ( 'NONE',  ( 1.224646799147343593E-16, 0.000000000000000000, -1.000000000000000000 ) ) ;
#1053 = EDGE_CURVE ( 'NONE', #8246, #3171, #4640, .T. ) ;
#1054 = ORIENTED_EDGE ( 'NONE', *, *, #4125, .T. ) ;
#1055 = FACE_OUTER_BOUND ( 'NONE', #5530, .T. ) ;
#1056 = ORIENTED_EDGE ( 'NONE', *, *, #8407, .F. ) ;
#1057 = ORIENTED_EDGE ( 'NONE', *, *, #10874, .T. ) ;
#1058 = LINE ( 'NONE', #7803, #11644 ) ;
#1059 = CARTESIAN_POINT ( 'NONE',  ( -0.5379290338433416752, -0.1023622047244094474, 0.2423824958184911116 ) ) ;
#1060 = CARTESIAN_POINT ( 'NONE',  ( -1.929388278599686757, -2.859527306003167624, -0.1546535441990251891 ) ) ;
#1061 = CARTESIAN_POINT ( 'NONE',  ( -1.365923773973335572E-16, 35.81796616381087262, 1.024442868901875804E-16 ) ) ;
#1062 = DIMENSIONAL_EXPONENTS ( 1.000000000000000000, 0.000000000000000000, 0.000000000000000000, 0.000000000000000000, 0.000000000000000000, 0.000000000000000000, 0.000000000000000000 ) ;
#1063 = CARTESIAN_POINT ( 'NONE',  ( -1.959562225762719878, -2.764756976402351185, -0.1771653543306641321 ) ) ;
#1064 = AXIS2_PLACEMENT_3D ( 'NONE', #11866, #5662, #15159 ) ;
#1065 = DIRECTION ( 'NONE',  ( 0.000000000000000000, 0.000000000000000000, 1.000000000000000000 ) ) ;
#1066 = CARTESIAN_POINT ( 'NONE',  ( 1.181102362204724310, 4.044111181948214319E-16, -0.02952755905511811330 ) ) ;
#1067 = FACE_OUTER_BOUND ( 'NONE', #9501, .T. ) ;
#1068 = EDGE_CURVE ( 'NONE', #14001, #14806, #7204, .T. ) ;
#1069 = FACE_OUTER_BOUND ( 'NONE', #2234, .T. ) ;
#1070 = DIRECTION ( 'NONE',  ( 0.000000000000000000, 0.000000000000000000, -1.000000000000000000 ) ) ;
#1071 = EDGE_CURVE ( 'NONE', #3617, #14001, #11, .T. ) ;
#1072 = EDGE_LOOP ( 'NONE', ( #11242, #14038, #2085, #1813 ) ) ;
#1073 = ORIENTED_EDGE ( 'NONE', *, *, #4324, .F. ) ;
#1074 = ORIENTED_EDGE ( 'NONE', *, *, #9322, .F. ) ;
#1075 = ORIENTED_EDGE ( 'NONE', *, *, #14521, .F. ) ;
#1076 = EDGE_CURVE ( 'NONE', #9943, #13968, #6081, .T. ) ;
#1077 =( BOUNDED_CURVE ( )  B_SPLINE_CURVE ( 3, ( #8250, #15379, #1045, #14277 ),
 .UNSPECIFIED., .F., .T. ) 
 B_SPLINE_CURVE_WITH_KNOTS ( ( 4, 4 ),
 ( 4.712388980384689674, 7.853981633974482790 ),
 .UNSPECIFIED. ) 
 CURVE ( )  GEOMETRIC_REPRESENTATION_ITEM ( )  RATIONAL_B_SPLINE_CURVE ( ( 1.000000000000000000, 0.3333333333333333703, 0.3333333333333333703, 1.000000000000000000 ) ) 
 REPRESENTATION_ITEM ( '' )  );
#1078 = DIRECTION ( 'NONE',  ( -0.000000000000000000, -2.212657494868377674E-16, -1.000000000000000000 ) ) ;
#1079 = CARTESIAN_POINT ( 'NONE',  ( 0.000000000000000000, -0.4881889763779528324, 0.2083147301385909200 ) ) ;
#1080 = FACE_OUTER_BOUND ( 'NONE', #2492, .T. ) ;
#1081 = DIRECTION ( 'NONE',  ( -0.4999999999999982236, 0.000000000000000000, -0.8660254037844395958 ) ) ;
#1082 = VECTOR ( 'NONE', #8513, 39.37007874015748143 ) ;
#1083 = VERTEX_POINT ( 'NONE', #4992 ) ;
#1084 = VECTOR ( 'NONE', #13829, 39.37007874015748143 ) ;
#1085 = DIRECTION ( 'NONE',  ( 0.000000000000000000, -1.000000000000000000, 0.000000000000000000 ) ) ;
#1086 = DIRECTION ( 'NONE',  ( -0.000000000000000000, -1.000000000000000000, -0.000000000000000000 ) ) ;
#1087 = EDGE_CURVE ( 'NONE', #1730, #1174, #1165, .T. ) ;
#1088 = TOROIDAL_SURFACE ( 'NONE', #12839, 0.007874015748031495954, 0.003937007874015747977 ) ;
#1089 = EDGE_CURVE ( 'NONE', #8213, #14839, #8903, .T. ) ;
#1090 = ORIENTED_EDGE ( 'NONE', *, *, #11951, .F. ) ;
#1091 = ORIENTED_EDGE ( 'NONE', *, *, #14062, .T. ) ;
#1092 = ADVANCED_FACE ( 'NONE', ( #13387 ), #3589, .T. ) ;
#1093 = VERTEX_POINT ( 'NONE', #6626 ) ;
#1094 = AXIS2_PLACEMENT_3D ( 'NONE', #3540, #10900, #6990 ) ;
#1095 = AXIS2_PLACEMENT_3D ( 'NONE', #3557, #11728, #2237 ) ;
#1096 = FACE_OUTER_BOUND ( 'NONE', #3085, .T. ) ;
#1097 = VECTOR ( 'NONE', #5408, 39.37007874015748143 ) ;
#1098 = AXIS2_PLACEMENT_3D ( 'NONE', #9093, #12777, #13874 ) ;
#1099 = CYLINDRICAL_SURFACE ( 'NONE', #1860, 0.1771653543307079026 ) ;
#1100 = LINE ( 'NONE', #13950, #15396 ) ;
#1101 = DIRECTION ( 'NONE',  ( -0.000000000000000000, 0.000000000000000000, 1.000000000000000000 ) ) ;
#1102 = CARTESIAN_POINT ( 'NONE',  ( -1.938117758475286001, -2.767509491613813655, 0.1578460832164983174 ) ) ;
#1103 = ORIENTED_EDGE ( 'NONE', *, *, #13036, .T. ) ;
#1104 = APPLICATION_CONTEXT ( 'automotive_design' ) ;
#1105 = CARTESIAN_POINT ( 'NONE',  ( -0.06692913385815728311, -0.2952755905511811330, -0.4190977005962941426 ) ) ;
#1106 = DIRECTION ( 'NONE',  ( -0.8660254037844385966, 0.000000000000000000, 0.5000000000000001110 ) ) ;
#1107 = AXIS2_PLACEMENT_3D ( 'NONE', #7484, #1611, #6375 ) ;
#1108 = CIRCLE ( 'NONE', #13108, 0.003937007874015758385 ) ;
#1109 = CARTESIAN_POINT ( 'NONE',  ( -0.4815353412745217998, 1.041793866378536437, 0.3474236500605538125 ) ) ;
#1110 = EDGE_CURVE ( 'NONE', #5248, #14646, #12526, .T. ) ;
#1111 = CARTESIAN_POINT ( 'NONE',  ( -1.598024000616091067, 0.1108860284103144050, 0.04651097583972436250 ) ) ;
#1112 = ORIENTED_EDGE ( 'NONE', *, *, #1196, .F. ) ;
#1113 = VECTOR ( 'NONE', #2240, 39.37007874015748143 ) ;
#1114 = AXIS2_PLACEMENT_3D ( 'NONE', #9732, #3997, #11107 ) ;
#1115 = VECTOR ( 'NONE', #15463, 39.37007874015748143 ) ;
#1116 = ORIENTED_EDGE ( 'NONE', *, *, #5872, .T. ) ;
#1117 = EDGE_CURVE ( 'NONE', #8847, #15055, #5351, .T. ) ;
#1118 = EDGE_LOOP ( 'NONE', ( #3689, #4152, #977, #3450 ) ) ;
#1119 = ORIENTED_EDGE ( 'NONE', *, *, #2493, .F. ) ;
#1120 = ORIENTED_EDGE ( 'NONE', *, *, #4380, .T. ) ;
#1121 = CARTESIAN_POINT ( 'NONE',  ( -0.4854723491485722353, 1.190944881889763884, 0.3484785681409914293 ) ) ;
#1122 = AXIS2_PLACEMENT_3D ( 'NONE', #14650, #2657, #6303 ) ;
#1123 = CIRCLE ( 'NONE', #15120, 0.003937007874015749712 ) ;
#1124 = AXIS2_PLACEMENT_3D ( 'NONE', #9247, #5475, #10193 ) ;
#1125 = EDGE_CURVE ( 'NONE', #5966, #5709, #132, .T. ) ;
#1126 = CARTESIAN_POINT ( 'NONE',  ( -1.607606114292111199, 0.09732815221480045631, -0.07874015748031495954 ) ) ;
#1127 = CARTESIAN_POINT ( 'NONE',  ( -0.09842519685028340570, -0.4881889763779528324, -0.5870514566507987197 ) ) ;
#1128 = AXIS2_PLACEMENT_3D ( 'NONE', #12813, #11885, #4676 ) ;
#1129 = CONTEXT_DEPENDENT_SHAPE_REPRESENTATION ( #6184, #6428 ) ;
#1130 = DIRECTION ( 'NONE',  ( -1.000000000000000000, 0.000000000000000000, 0.000000000000000000 ) ) ;
#1131 = CIRCLE ( 'NONE', #119, 0.003937007874015758385 ) ;
#1132 = DIRECTION ( 'NONE',  ( 0.000000000000000000, -1.000000000000000000, 0.000000000000000000 ) ) ;
#1133 = DIRECTION ( 'NONE',  ( -1.000000000000000000, 0.000000000000000000, 0.000000000000000000 ) ) ;
#1134 = EDGE_LOOP ( 'NONE', ( #4813, #11868, #6038, #12518 ) ) ;
#1135 = CARTESIAN_POINT ( 'NONE',  ( -1.596293587998450780, 0.1133155780026439408, -0.04477369844320916448 ) ) ;
#1136 = CARTESIAN_POINT ( 'NONE',  ( 0.4591888763630541104, -0.1023622047244094474, 0.3787644491703230365 ) ) ;
#1137 = DIRECTION ( 'NONE',  ( 0.9926610512904576744, 0.1209298856814283729, -0.000000000000000000 ) ) ;
#1138 = AXIS2_PLACEMENT_3D ( 'NONE', #9344, #11618, #1048 ) ;
#1139 = CIRCLE ( 'NONE', #12894, 2.214566929133857887 ) ;
#1140 = AXIS2_PLACEMENT_3D ( 'NONE', #5537, #11445, #11679 ) ;
#1141 = ORIENTED_EDGE ( 'NONE', *, *, #10199, .F. ) ;
#1142 = ORIENTED_EDGE ( 'NONE', *, *, #7498, .T. ) ;
#1143 = ORIENTED_EDGE ( 'NONE', *, *, #5974, .F. ) ;
#1144 = CIRCLE ( 'NONE', #11897, 0.007874015748031516770 ) ;
#1145 = EDGE_LOOP ( 'NONE', ( #3197, #1402, #14727 ) ) ;
#1146 = ORIENTED_EDGE ( 'NONE', *, *, #3577, .T. ) ;
#1147 = CARTESIAN_POINT ( 'NONE',  ( 1.181102362204724310, 4.044111181948214319E-16, -0.02559055118110236185 ) ) ;
#1148 = EDGE_CURVE ( 'NONE', #11634, #8246, #13667, .T. ) ;
#1149 = DIRECTION ( 'NONE',  ( 0.000000000000000000, 0.000000000000000000, 1.000000000000000000 ) ) ;
#1150 = CARTESIAN_POINT ( 'NONE',  ( -1.939652992539211640, -2.828352525160966024, 0.1684558939921211862 ) ) ;
#1151 =( NAMED_UNIT ( * ) PLANE_ANGLE_UNIT ( ) SI_UNIT ( $, .RADIAN. ) );
#1152 = AXIS2_PLACEMENT_3D ( 'NONE', #15103, #770, #15035 ) ;
#1153 = LINE ( 'NONE', #11731, #4595 ) ;
#1154 = CIRCLE ( 'NONE', #1885, 0.007874015748031499423 ) ;
#1155 = CIRCLE ( 'NONE', #3137, 0.007874015748031516770 ) ;
#1156 = CARTESIAN_POINT ( 'NONE',  ( 0.2364476915724980366, -0.1023622047244094474, 0.06377609659104091500 ) ) ;
#1157 = FACE_OUTER_BOUND ( 'NONE', #5396, .T. ) ;
#1158 = TOROIDAL_SURFACE ( 'NONE', #8388, 0.04330708661417329020, 0.003937007874015747977 ) ;
#1159 = DIRECTION ( 'NONE',  ( -0.000000000000000000, 1.000000000000000000, -0.000000000000000000 ) ) ;
#1160 = ORIENTED_EDGE ( 'NONE', *, *, #14997, .F. ) ;
#1161 = ORIENTED_EDGE ( 'NONE', *, *, #8660, .F. ) ;
#1162 = CIRCLE ( 'NONE', #14161, 0.003937007874015749712 ) ;
#1163 = VERTEX_POINT ( 'NONE', #1637 ) ;
#1164 = CIRCLE ( 'NONE', #7652, 2.795275590551181466 ) ;
#1165 = CIRCLE ( 'NONE', #408, 0.04527559055118110520 ) ;
#1166 = VERTEX_POINT ( 'NONE', #12290 ) ;
#1167 = AXIS2_PLACEMENT_3D ( 'NONE', #6938, #6845, #4745 ) ;
#1168 = CARTESIAN_POINT ( 'NONE',  ( -0.5418660417173573052, -0.4881889763779528324, 0.2355633981508970798 ) ) ;
#1169 = CARTESIAN_POINT ( 'NONE',  ( -0.02344272421052690653, 0.1505984473678075031, 0.03705048130897044961 ) ) ;
#1170 = DIRECTION ( 'NONE',  ( -1.000000000000000000, 0.000000000000000000, 0.000000000000000000 ) ) ;
#1171 = DIRECTION ( 'NONE',  ( 0.8660254037844431485, 0.000000000000000000, 0.4999999999999918954 ) ) ;
#1172 = AXIS2_PLACEMENT_3D ( 'NONE', #8430, #6053, #10842 ) ;
#1173 = DIRECTION ( 'NONE',  ( -3.614007241618347785E-16, 0.000000000000000000, 1.000000000000000000 ) ) ;
#1174 = VERTEX_POINT ( 'NONE', #617 ) ;
#1175 = EDGE_CURVE ( 'NONE', #10209, #7182, #169, .T. ) ;
#1176 = FACE_OUTER_BOUND ( 'NONE', #14953, .T. ) ;
#1177 = CARTESIAN_POINT ( 'NONE',  ( -0.4591888763630546655, -0.1023622047244094474, 0.3787644491703233141 ) ) ;
#1178 = CIRCLE ( 'NONE', #423, 0.003937007874015721089 ) ;
#1179 = ORIENTED_EDGE ( 'NONE', *, *, #8976, .T. ) ;
#1180 = VERTEX_POINT ( 'NONE', #1787 ) ;
#1181 = ORIENTED_EDGE ( 'NONE', *, *, #12010, .F. ) ;
#1182 = CIRCLE ( 'NONE', #3924, 0.01968503937007875723 ) ;
#1183 = CARTESIAN_POINT ( 'NONE',  ( 0.4330708661417309036, -0.09448818897637796532, 0.4318761856142889766 ) ) ;
#1184 = EDGE_CURVE ( 'NONE', #2378, #12957, #5055, .T. ) ;
#1185 = DIRECTION ( 'NONE',  ( -0.8144815189573203495, 0.5801894994542524664, -0.000000000000000000 ) ) ;
#1186 = CARTESIAN_POINT ( 'NONE',  ( -1.927081998786787986, -2.943867889510814795, 0.04476392992596674864 ) ) ;
#1187 = CIRCLE ( 'NONE', #14183, 0.01968503937007875723 ) ;
#1188 = EDGE_CURVE ( 'NONE', #6757, #2760, #6860, .T. ) ;
#1189 = DIRECTION ( 'NONE',  ( -0.4999999999999979461, -0.000000000000000000, -0.8660254037844398178 ) ) ;
#1190 = CARTESIAN_POINT ( 'NONE',  ( 0.9851651268172137987, -1.725292181286280480, 0.1968503937007874127 ) ) ;
#1191 = DIRECTION ( 'NONE',  ( -0.8660254037844385966, 0.000000000000000000, 0.5000000000000001110 ) ) ;
#1192 = CARTESIAN_POINT ( 'NONE',  ( -0.6864776960422505070, 1.190944881889763884, 0.4645290592786119332 ) ) ;
#1193 = CARTESIAN_POINT ( 'NONE',  ( -1.945358927863352072, -2.810530894188501883, 0.1731069454022728660 ) ) ;
#1194 = EDGE_LOOP ( 'NONE', ( #138, #12948, #905, #1357 ) ) ;
#1195 = CARTESIAN_POINT ( 'NONE',  ( -1.947553218330493774, -2.926780783575864131, -0.05681056732657507186 ) ) ;
#1196 = EDGE_CURVE ( 'NONE', #10513, #12909, #476, .T. ) ;
#1197 = DIRECTION ( 'NONE',  ( 0.8660254037844362651, 4.956352788505159323E-16, -0.5000000000000041078 ) ) ;
#1198 = FACE_BOUND ( 'NONE', #8594, .T. ) ;
#1199 = CARTESIAN_POINT ( 'NONE',  ( -0.5860051159906336515, -0.003937007874015747977, 0.1591122789105256785 ) ) ;
#1200 = ORIENTED_EDGE ( 'NONE', *, *, #4816, .T. ) ;
#1201 = AXIS2_PLACEMENT_3D ( 'NONE', #12954, #2288, #9341 ) ;
#1202 = VERTEX_POINT ( 'NONE', #10085 ) ;
#1203 = DIRECTION ( 'NONE',  ( 0.000000000000000000, 1.000000000000000000, 0.000000000000000000 ) ) ;
#1204 = ADVANCED_FACE ( 'NONE', ( #307 ), #13467, .T. ) ;
#1205 = DIRECTION ( 'NONE',  ( 0.000000000000000000, 0.000000000000000000, -1.000000000000000000 ) ) ;
#1206 = TOROIDAL_SURFACE ( 'NONE', #3702, 0.04330708661417329020, 0.003937007874015747977 ) ;
#1207 = ADVANCED_FACE ( 'NONE', ( #8928 ), #5376, .T. ) ;
#1208 = CARTESIAN_POINT ( 'NONE',  ( -1.596293587998450780, 0.1133155780026439408, -0.04477369844320916448 ) ) ;
#1209 = DIRECTION ( 'NONE',  ( 0.5000000000000036637, -0.000000000000000000, 0.8660254037844364872 ) ) ;
#1210 = AXIS2_PLACEMENT_3D ( 'NONE', #11174, #13373, #11016 ) ;
#1211 = DIRECTION ( 'NONE',  ( -1.000000000000000000, -4.565061778886334044E-16, 0.000000000000000000 ) ) ;
#1212 = ORIENTED_EDGE ( 'NONE', *, *, #12986, .T. ) ;
#1213 = DIRECTION ( 'NONE',  ( 0.000000000000000000, 0.000000000000000000, 1.000000000000000000 ) ) ;
#1214 = EDGE_CURVE ( 'NONE', #11540, #7421, #7608, .T. ) ;
#1215 = LINE ( 'NONE', #4873, #10383 ) ;
#1216 = FACE_BOUND ( 'NONE', #3530, .T. ) ;
#1217 = LINE ( 'NONE', #5970, #5418 ) ;
#1218 = AXIS2_PLACEMENT_3D ( 'NONE', #2988, #6561, #6799 ) ;
#1219 = ORIENTED_EDGE ( 'NONE', *, *, #2551, .T. ) ;
#1220 = ORIENTED_EDGE ( 'NONE', *, *, #14480, .F. ) ;
#1221 = ORIENTED_EDGE ( 'NONE', *, *, #14388, .F. ) ;
#1222 = AXIS2_PLACEMENT_3D ( 'NONE', #4060, #6407, #9963 ) ;
#1223 = VERTEX_POINT ( 'NONE', #14796 ) ;
#1224 = DIRECTION ( 'NONE',  ( -0.8660254037844383745, 0.000000000000000000, -0.5000000000000004441 ) ) ;
#1225 = CARTESIAN_POINT ( 'NONE',  ( -0.5445274672588088505, 1.043307086614173373, 0.2461921031270815907 ) ) ;
#1226 = FACE_OUTER_BOUND ( 'NONE', #2353, .T. ) ;
#1227 = CARTESIAN_POINT ( 'NONE',  ( 1.296919926260489131, 35.08612325493803041, 0.5442041385160382161 ) ) ;
#1228 = PLANE ( 'NONE',  #854 ) ;
#1229 = CIRCLE ( 'NONE', #15232, 0.003937007874015721089 ) ;
#1230 = CARTESIAN_POINT ( 'NONE',  ( 4.821444091131311524E-18, 0.4133858267716535306, 0.03937007874015747977 ) ) ;
#1231 = CARTESIAN_POINT ( 'NONE',  ( 0.000000000000000000, 2.637795275590551825, 0.03937007874015747977 ) ) ;
#1232 = DIRECTION ( 'NONE',  ( 0.000000000000000000, 0.000000000000000000, 1.000000000000000000 ) ) ;
#1233 = EDGE_CURVE ( 'NONE', #11698, #12320, #6903, .T. ) ;
#1234 = CARTESIAN_POINT ( 'NONE',  ( 0.1022864650139100745, 0.05905511811023622659, 1.563012696487738457E-17 ) ) ;
#1235 = AXIS2_PLACEMENT_3D ( 'NONE', #4705, #6890, #5944 ) ;
#1236 = EDGE_CURVE ( 'NONE', #8739, #5216, #8622, .T. ) ;
#1237 = ORIENTED_EDGE ( 'NONE', *, *, #15345, .T. ) ;
#1238 = EDGE_CURVE ( 'NONE', #3335, #15025, #11109, .T. ) ;
#1239 = ORIENTED_EDGE ( 'NONE', *, *, #359, .T. ) ;
#1240 = ORIENTED_EDGE ( 'NONE', *, *, #15271, .F. ) ;
#1241 = ORIENTED_EDGE ( 'NONE', *, *, #1117, .T. ) ;
#1242 = CARTESIAN_POINT ( 'NONE',  ( -2.107117561417118701, -2.011956994529711995, -0.1111970799389148945 ) ) ;
#1243 = CARTESIAN_POINT ( 'NONE',  ( -0.1181102362204724254, 2.448818897637795367, 0.03937007874015747977 ) ) ;
#1244 = CYLINDRICAL_SURFACE ( 'NONE', #10211, 0.003937007874015758385 ) ;
#1245 = FACE_OUTER_BOUND ( 'NONE', #4224, .T. ) ;
#1246 = DIRECTION ( 'NONE',  ( 1.000000000000000000, 0.000000000000000000, -1.224646799147353207E-16 ) ) ;
#1247 = DIRECTION ( 'NONE',  ( 0.000000000000000000, 1.000000000000000000, 0.000000000000000000 ) ) ;
#1248 = EDGE_LOOP ( 'NONE', ( #7093, #11274, #11913, #12025 ) ) ;
#1249 = FILL_AREA_STYLE ('',( #9480 ) ) ;
#1250 = DIRECTION ( 'NONE',  ( 0.000000000000000000, 1.000000000000000000, 0.000000000000000000 ) ) ;
#1251 = LINE ( 'NONE', #6004, #13665 ) ;
#1252 = ORIENTED_EDGE ( 'NONE', *, *, #1964, .F. ) ;
#1253 = EDGE_LOOP ( 'NONE', ( #3177, #2084, #3195, #11288 ) ) ;
#1254 = VERTEX_POINT ( 'NONE', #3910 ) ;
#1255 = CARTESIAN_POINT ( 'NONE',  ( -0.05905511811012585655, -0.1023622047244094474, -0.5870514566507987197 ) ) ;
#1256 = CARTESIAN_POINT ( 'NONE',  ( -0.4749369078591176296, -0.4881889763779528324, 0.3514880584999472424 ) ) ;
#1257 = CARTESIAN_POINT ( 'NONE',  ( -0.02018259705034725071, -0.1802452534892125813, 1.049219007154695292E-17 ) ) ;
#1258 = DIRECTION ( 'NONE',  ( -0.000000000000000000, -0.000000000000000000, -1.000000000000000000 ) ) ;
#1259 = CARTESIAN_POINT ( 'NONE',  ( 5.544660704801008561E-18, 0.06496062992125986590, -0.04527559055118110520 ) ) ;
#1260 = ORIENTED_EDGE ( 'NONE', *, *, #2805, .T. ) ;
#1261 = CARTESIAN_POINT ( 'NONE',  ( -1.943861602385431375, -2.935750972982893447, 0.02297894316446263269 ) ) ;
#1262 = LINE ( 'NONE', #8158, #5344 ) ;
#1263 = DIRECTION ( 'NONE',  ( 1.349229370204184172E-15, 1.000000000000000000, 0.000000000000000000 ) ) ;
#1264 = ORIENTED_EDGE ( 'NONE', *, *, #10230, .T. ) ;
#1265 = EDGE_CURVE ( 'NONE', #5839, #2421, #2621, .T. ) ;
#1266 = B_SPLINE_CURVE_WITH_KNOTS ( 'NONE', 3,
 ( #12133, #3899, #13522, #2644 ),
 .UNSPECIFIED., .F., .F.,
 ( 4, 4 ),
 ( 0.0002461255424396390835, 0.0003583013531701043780 ),
 .UNSPECIFIED. ) ;
#1267 = ORIENTED_EDGE ( 'NONE', *, *, #5390, .F. ) ;
#1268 = EDGE_CURVE ( 'NONE', #14809, #9393, #13378, .T. ) ;
#1269 = PRODUCT_DEFINITION_CONTEXT ( 'detailed design', #7577, 'design' ) ;
#1270 = ORIENTED_EDGE ( 'NONE', *, *, #2028, .T. ) ;
#1271 = DIRECTION ( 'NONE',  ( -3.614007241618347785E-16, 0.000000000000000000, 1.000000000000000000 ) ) ;
#1272 = ADVANCED_FACE ( 'NONE', ( #12912 ), #7893, .F. ) ;
#1273 = CARTESIAN_POINT ( 'NONE',  ( -0.05114323250695503725, 0.000000000000000000, -0.08858267716535432601 ) ) ;
#1274 = DIRECTION ( 'NONE',  ( 0.000000000000000000, 0.000000000000000000, -1.000000000000000000 ) ) ;
#1275 = CARTESIAN_POINT ( 'NONE',  ( -1.181102362204724310, 0.000000000000000000, 0.02952755905511811330 ) ) ;
#1276 = CARTESIAN_POINT ( 'NONE',  ( 1.224409448818897461, 4.044111181948214319E-16, -0.02952755905511811330 ) ) ;
#1277 = DIRECTION ( 'NONE',  ( -0.000000000000000000, -1.000000000000000000, -0.000000000000000000 ) ) ;
#1278 = CARTESIAN_POINT ( 'NONE',  ( -3.379785373986829049E-18, 1.043307086614173596, 1.951319995474476809E-18 ) ) ;
#1279 = ORIENTED_EDGE ( 'NONE', *, *, #2460, .T. ) ;
#1280 = CARTESIAN_POINT ( 'NONE',  ( 0.5894146648244296127, -0.09448818897637796532, 0.1571437749735214717 ) ) ;
#1281 = DIRECTION ( 'NONE',  ( -0.4999999999999996114, -0.000000000000000000, -0.8660254037844389297 ) ) ;
#1282 = CARTESIAN_POINT ( 'NONE',  ( 0.000000000000000000, 1.346456692913385877, 0.000000000000000000 ) ) ;
#1283 = EDGE_CURVE ( 'NONE', #14180, #10993, #4357, .T. ) ;
#1284 = DIRECTION ( 'NONE',  ( 1.000000000000000000, 0.000000000000000000, 0.000000000000000000 ) ) ;
#1285 = ADVANCED_FACE ( 'NONE', ( #6953 ), #1946, .T. ) ;
#1286 = ORIENTED_EDGE ( 'NONE', *, *, #2735, .F. ) ;
#1287 = ORIENTED_EDGE ( 'NONE', *, *, #1175, .T. ) ;
#1288 = ORIENTED_EDGE ( 'NONE', *, *, #11461, .T. ) ;
#1289 = VERTEX_POINT ( 'NONE', #12821 ) ;
#1290 = EDGE_CURVE ( 'NONE', #532, #10983, #3267, .T. ) ;
#1291 = DIRECTION ( 'NONE',  ( -0.8660254037844405950, 0.000000000000000000, -0.4999999999999966693 ) ) ;
#1292 = CARTESIAN_POINT ( 'NONE',  ( 0.000000000000000000, 0.003937007874015749712, 0.04330708661417326938 ) ) ;
#1293 = CARTESIAN_POINT ( 'NONE',  ( -1.939653092248158073, -2.828352430279280405, -0.1684573650302815528 ) ) ;
#1294 = DIRECTION ( 'NONE',  ( -1.000000000000000000, 2.826464243713527219E-17, 6.933134904822705894E-16 ) ) ;
#1295 = CARTESIAN_POINT ( 'NONE',  ( 0.3569402812043664941, -0.2952755905511811330, 0.1333425256503553147 ) ) ;
#1296 = PLANE ( 'NONE',  #7157 ) ;
#1297 = CARTESIAN_POINT ( 'NONE',  ( -1.511943070284283097, 0.2262540267724839904, -0.03937007874015747977 ) ) ;
#1298 = PLANE ( 'NONE',  #5602 ) ;
#1299 = DIRECTION ( 'NONE',  ( 1.000000000000000000, 0.000000000000000000, 0.000000000000000000 ) ) ;
#1300 = CARTESIAN_POINT ( 'NONE',  ( 0.04921259842516963884, -0.4881889763779528324, -0.08523872084487790768 ) ) ;
#1301 = EDGE_CURVE ( 'NONE', #4570, #1083, #3621, .T. ) ;
#1302 = VERTEX_POINT ( 'NONE', #10404 ) ;
#1303 = EDGE_LOOP ( 'NONE', ( #7238, #14934, #10727, #5233 ) ) ;
#1304 = ORIENTED_EDGE ( 'NONE', *, *, #12115, .T. ) ;
#1305 = EDGE_CURVE ( 'NONE', #4499, #5085, #10411, .T. ) ;
#1306 = EDGE_CURVE ( 'NONE', #13646, #13558, #2180, .T. ) ;
#1307 = CARTESIAN_POINT ( 'NONE',  ( -2.110117738960459732, -1.869206010357609138, -0.1064927656600950512 ) ) ;
#1308 = DIRECTION ( 'NONE',  ( 0.000000000000000000, 1.000000000000000000, 0.000000000000000000 ) ) ;
#1309 = CYLINDRICAL_SURFACE ( 'NONE', #14469, 0.003937007874015737569 ) ;
#1310 = EDGE_CURVE ( 'NONE', #10983, #14128, #2903, .T. ) ;
#1311 = CARTESIAN_POINT ( 'NONE',  ( -0.5905511811023629321, -0.09842519685039370636, 0.1591122789105256785 ) ) ;
#1312 = CARTESIAN_POINT ( 'NONE',  ( -0.4591888763630546655, -0.4881889763779528324, 0.3787644491703233141 ) ) ;
#1313 = CYLINDRICAL_SURFACE ( 'NONE', #6115, 0.05905511811023625435 ) ;
#1314 =( NAMED_UNIT ( * ) SI_UNIT ( $, .STERADIAN. ) SOLID_ANGLE_UNIT ( ) );
#1315 = CARTESIAN_POINT ( 'NONE',  ( 0.06012952712669447641, 1.340161268289288499, -0.5902914708161598467 ) ) ;
#1316 = CARTESIAN_POINT ( 'NONE',  ( 0.4854723491485768982, 1.043263280880422528, 0.3484785681409844904 ) ) ;
#1317 = ORIENTED_EDGE ( 'NONE', *, *, #8054, .T. ) ;
#1318 = ORIENTED_EDGE ( 'NONE', *, *, #13456, .T. ) ;
#1319 = ORIENTED_EDGE ( 'NONE', *, *, #8741, .T. ) ;
#1320 = LINE ( 'NONE', #7337, #8879 ) ;
#1321 = CARTESIAN_POINT ( 'NONE',  ( -1.063205505495480097, 0.7941372572243097228, -0.05905511811023622659 ) ) ;
#1322 = DIRECTION ( 'NONE',  ( -0.8660254037844385966, -0.000000000000000000, 0.4999999999999998890 ) ) ;
#1323 = ADVANCED_FACE ( 'NONE', ( #12756 ), #15183, .T. ) ;
#1324 = LINE ( 'NONE', #7431, #6350 ) ;
#1325 = CARTESIAN_POINT ( 'NONE',  ( -2.099929645851249305, -2.385360057864538419, 0.1341722008959284895 ) ) ;
#1326 = DIRECTION ( 'NONE',  ( 0.000000000000000000, 0.000000000000000000, -1.000000000000000000 ) ) ;
#1327 = CARTESIAN_POINT ( 'NONE',  ( -1.908398435458060760, -2.849708334410140154, 0.1334289122196857802 ) ) ;
#1328 = EDGE_LOOP ( 'NONE', ( #10548, #501, #5156, #7523, #3720 ) ) ;
#1329 = LINE ( 'NONE', #4937, #2425 ) ;
#1330 = CARTESIAN_POINT ( 'NONE',  ( 0.000000000000000000, 2.637795275590551825, -0.03937007874015747977 ) ) ;
#1331 = ORIENTED_EDGE ( 'NONE', *, *, #14763, .F. ) ;
#1332 = ORIENTED_EDGE ( 'NONE', *, *, #9121, .T. ) ;
#1333 = AXIS2_PLACEMENT_3D ( 'NONE', #4553, #3474, #8247 ) ;
#1334 = AXIS2_PLACEMENT_3D ( 'NONE', #2347, #7133, #2089 ) ;
#1335 = AXIS2_PLACEMENT_3D ( 'NONE', #10250, #13616, #7667 ) ;
#1336 = ORIENTED_EDGE ( 'NONE', *, *, #878, .F. ) ;
#1337 = DIRECTION ( 'NONE',  ( -0.000000000000000000, -1.000000000000000000, -0.000000000000000000 ) ) ;
#1338 = LINE ( 'NONE', #10588, #342 ) ;
#1339 = DIRECTION ( 'NONE',  ( -0.000000000000000000, -1.000000000000000000, -0.000000000000000000 ) ) ;
#1340 = CARTESIAN_POINT ( 'NONE',  ( 0.5452755905511544876, -0.1023622047244094474, 0.2375319020879054499 ) ) ;
#1341 = CARTESIAN_POINT ( 'NONE',  ( -0.03886060139087894189, 0.06736074103232447818, -0.08219815605944147396 ) ) ;
#1342 = CIRCLE ( 'NONE', #2831, 0.007874015748031475137 ) ;
#1343 = CARTESIAN_POINT ( 'NONE',  ( 0.6864776960422569463, 1.190944881889763884, 0.4645290592786023298 ) ) ;
#1344 = AXIS2_PLACEMENT_3D ( 'NONE', #14460, #10919, #11875 ) ;
#1345 = CARTESIAN_POINT ( 'NONE',  ( -0.03802712947489396422, 0.1704066588063142818, -0.02158149019474813607 ) ) ;
#1346 = ORIENTED_EDGE ( 'NONE', *, *, #10688, .T. ) ;
#1347 = CARTESIAN_POINT ( 'NONE',  ( -1.596214514713377719, 0.1135332889814023166, -0.07874015748031495954 ) ) ;
#1348 = TOROIDAL_SURFACE ( 'NONE', #1848, 0.5984251968503937480, 0.007874015748031495954 ) ;
#1349 = TOROIDAL_SURFACE ( 'NONE', #603, 0.6614173228346456046, 0.007874015748031495954 ) ;
#1350 = LINE ( 'NONE', #2370, #3127 ) ;
#1351 = DIRECTION ( 'NONE',  ( 0.000000000000000000, -0.000000000000000000, 1.000000000000000000 ) ) ;
#1352 = EDGE_CURVE ( 'NONE', #2681, #1223, #2011, .T. ) ;
#1353 = CYLINDRICAL_SURFACE ( 'NONE', #4678, 0.03937007874015754916 ) ;
#1354 = ORIENTED_EDGE ( 'NONE', *, *, #9263, .F. ) ;
#1355 = ORIENTED_EDGE ( 'NONE', *, *, #11027, .T. ) ;
#1357 = ORIENTED_EDGE ( 'NONE', *, *, #4601, .F. ) ;
#1356 = AXIS2_PLACEMENT_3D ( 'NONE', #126, #9595, #13274 ) ;
#1358 = AXIS2_PLACEMENT_3D ( 'NONE', #1044, #9743, #14511 ) ;
#1359 = ORIENTED_EDGE ( 'NONE', *, *, #4172, .T. ) ;
#1360=STYLED_ITEM('',(#15505),#4199);
#1361 = AXIS2_PLACEMENT_3D ( 'NONE', #12006, #8303, #6896 ) ;
#1362 = CARTESIAN_POINT ( 'NONE',  ( 0.000000000000000000, 1.409448818897637956, 0.000000000000000000 ) ) ;
#1363 = CIRCLE ( 'NONE', #5850, 0.003937007874015721089 ) ;
#1364 = PRODUCT_DEFINITION_FORMATION_WITH_SPECIFIED_SOURCE ( 'ANY', '', #309, .NOT_KNOWN. ) ;
#1365 = CYLINDRICAL_SURFACE ( 'NONE', #9860, 0.003937007874015758385 ) ;
#1366 = FACE_OUTER_BOUND ( 'NONE', #3882, .T. ) ;
#1367 = EDGE_CURVE ( 'NONE', #11240, #7731, #4621, .T. ) ;
#1368 = DIRECTION ( 'NONE',  ( 0.7118260687460286062, 0.5695655044020486724, -0.4109729724067190948 ) ) ;
#1369 = DIRECTION ( 'NONE',  ( 0.000000000000000000, 1.000000000000000000, 0.000000000000000000 ) ) ;
#1370 = EDGE_CURVE ( 'NONE', #5863, #7929, #9298, .T. ) ;
#1371 = CARTESIAN_POINT ( 'NONE',  ( 0.000000000000000000, 1.425196850393700920, 0.000000000000000000 ) ) ;
#1372 = CARTESIAN_POINT ( 'NONE',  ( -0.5860051159906336515, -0.003937007874015747977, 0.1591122789105256785 ) ) ;
#1373 = DIRECTION ( 'NONE',  ( 0.1408070410764336311, -0.9900370584898827708, 0.000000000000000000 ) ) ;
#1374 = AXIS2_PLACEMENT_3D ( 'NONE', #14211, #4317, #888 ) ;
#1375 = AXIS2_PLACEMENT_3D ( 'NONE', #2969, #8829, #12452 ) ;
#1376 = CIRCLE ( 'NONE', #9648, 0.1574803149606299191 ) ;
#1377 = AXIS2_PLACEMENT_3D ( 'NONE', #6098, #12073, #14573 ) ;
#1378 = ADVANCED_FACE ( 'NONE', ( #11423, #700 ), #5457, .F. ) ;
#1379 = DIRECTION ( 'NONE',  ( 0.000000000000000000, 0.000000000000000000, 1.000000000000000000 ) ) ;
#1380 = LINE ( 'NONE', #6140, #6914 ) ;
#1381 = CIRCLE ( 'NONE', #2120, 0.007874015748031482076 ) ;
#1382 = EDGE_LOOP ( 'NONE', ( #1200, #6636, #5665, #4463 ) ) ;
#1383 = ORIENTED_EDGE ( 'NONE', *, *, #10764, .F. ) ;
#1384 = EDGE_LOOP ( 'NONE', ( #10062, #14363 ) ) ;
#1385 = AXIS2_PLACEMENT_3D ( 'NONE', #11855, #1132, #8316 ) ;
#1386 = VECTOR ( 'NONE', #14931, 39.37007874015748143 ) ;
#1387 = AXIS2_PLACEMENT_3D ( 'NONE', #2383, #14228, #11795 ) ;
#1388 = EDGE_CURVE ( 'NONE', #7994, #5246, #4279, .T. ) ;
#1389 = DIRECTION ( 'NONE',  ( -1.000000000000000000, 0.000000000000000000, 0.000000000000000000 ) ) ;
#1390 = CARTESIAN_POINT ( 'NONE',  ( -1.607606114292111199, 0.09732815221480045631, 0.1968503937007874127 ) ) ;
#1391 = AXIS2_PLACEMENT_3D ( 'NONE', #4365, #6870, #2183 ) ;
#1392 = ADVANCED_FACE ( 'NONE', ( #11483 ), #15012, .T. ) ;
#1393 = DIRECTION ( 'NONE',  ( 0.000000000000000000, -0.000000000000000000, 1.000000000000000000 ) ) ;
#1394 = CARTESIAN_POINT ( 'NONE',  ( 0.4330708661417309036, -0.09842519685039370636, 0.4318761856142889766 ) ) ;
#1395 = DIRECTION ( 'NONE',  ( -0.5750876580239486779, -0.8180917953313858737, 4.257489128596104324E-15 ) ) ;
#1396 = DIRECTION ( 'NONE',  ( 0.4274092037376936992, 0.000000000000000000, 0.9040582794047684612 ) ) ;
#1397 = EDGE_CURVE ( 'NONE', #10200, #13984, #12426, .T. ) ;
#1398 = FACE_OUTER_BOUND ( 'NONE', #3786, .T. ) ;
#1399 = DIRECTION ( 'NONE',  ( 0.000000000000000000, 0.000000000000000000, -1.000000000000000000 ) ) ;
#1400 = VECTOR ( 'NONE', #8450, 39.37007874015748143 ) ;
#1401 = AXIS2_PLACEMENT_3D ( 'NONE', #3237, #8007, #11780 ) ;
#1402 = ORIENTED_EDGE ( 'NONE', *, *, #8846, .T. ) ;
#1403 = ORIENTED_EDGE ( 'NONE', *, *, #8453, .F. ) ;
#1404 = EDGE_LOOP ( 'NONE', ( #7999, #8474, #11179, #13109 ) ) ;
#1405 = VECTOR ( 'NONE', #11986, 39.37007874015748143 ) ;
#1406 = ORIENTED_EDGE ( 'NONE', *, *, #6368, .F. ) ;
#1407 =( REPRESENTATION_RELATIONSHIP ('NONE','NONE', #8904, #2403 ) REPRESENTATION_RELATIONSHIP_WITH_TRANSFORMATION ( #9340 )SHAPE_REPRESENTATION_RELATIONSHIP( ) );
#1408 = EDGE_CURVE ( 'NONE', #12754, #11565, #12138, .T. ) ;
#1409 = EDGE_LOOP ( 'NONE', ( #10744, #181, #7674, #8724 ) ) ;
#1410 = CARTESIAN_POINT ( 'NONE',  ( -2.163017314575554462, -1.630597114118274238, 0.1033464566929129663 ) ) ;
#1411 = CIRCLE ( 'NONE', #11413, 0.007874015748031482076 ) ;
#1412 = AXIS2_PLACEMENT_3D ( 'NONE', #3432, #14237, #13126 ) ;
#1413 = CYLINDRICAL_SURFACE ( 'NONE', #14624, 0.03937007874015751446 ) ;
#1414 = CARTESIAN_POINT ( 'NONE',  ( -0.04711866733795024020, -0.1840656518295272215, -0.03212400068286348082 ) ) ;
#1415 = FACE_OUTER_BOUND ( 'NONE', #2478, .T. ) ;
#1416 = DIRECTION ( 'NONE',  ( 0.000000000000000000, 0.000000000000000000, -1.000000000000000000 ) ) ;
#1417 = AXIS2_PLACEMENT_3D ( 'NONE', #7709, #14768, #573 ) ;
#1418 = CARTESIAN_POINT ( 'NONE',  ( -1.881677119634339812, -2.917705953332184965, -0.1022915504730082664 ) ) ;
#1419 = ORIENTED_EDGE ( 'NONE', *, *, #14159, .F. ) ;
#1420 = CARTESIAN_POINT ( 'NONE',  ( 1.181102362204724310, -0.1279527559055113062, -0.02559055118110236185 ) ) ;
#1421 = CARTESIAN_POINT ( 'NONE',  ( 0.5412478373021326616, 1.035433070866141891, 0.2362233606508025163 ) ) ;
#1422 = ADVANCED_FACE ( 'NONE', ( #5197 ), #5434, .T. ) ;
#1423 = DIRECTION ( 'NONE',  ( -0.8660254037844383745, 0.000000000000000000, -0.5000000000000004441 ) ) ;
#1424 = ORIENTED_EDGE ( 'NONE', *, *, #4740, .F. ) ;
#1425 = ORIENTED_EDGE ( 'NONE', *, *, #7203, .F. ) ;
#1426 = EDGE_CURVE ( 'NONE', #13559, #6292, #7633, .T. ) ;
#1427 = EDGE_CURVE ( 'NONE', #3491, #5898, #12416, .T. ) ;
#1428 = VERTEX_POINT ( 'NONE', #10228 ) ;
#1429 = CARTESIAN_POINT ( 'NONE',  ( 0.3706061991976991044, -0.09842519685039370636, -0.2139695888701345916 ) ) ;
#1430 = CARTESIAN_POINT ( 'NONE',  ( 0.000000000000000000, 1.346456692913385877, -0.5905511811023621549 ) ) ;
#1431 = LINE ( 'NONE', #6185, #1604 ) ;
#1432 = CARTESIAN_POINT ( 'NONE',  ( -0.2362204724409448231, -0.02638708502139245488, -0.05905511811023622659 ) ) ;
#1434 = AXIS2_PLACEMENT_3D ( 'NONE', #3064, #13735, #12317 ) ;
#1433 = CARTESIAN_POINT ( 'NONE',  ( 6.653592845761209348E-17, 0.04724409448818898960, 0.5433070866141731514 ) ) ;
#1435 = DIRECTION ( 'NONE',  ( -0.5000000000000000000, 0.000000000000000000, -0.8660254037844385966 ) ) ;
#1436 = VERTEX_POINT ( 'NONE', #5263 ) ;
#1437 = CARTESIAN_POINT ( 'NONE',  ( -0.4606299212598433113, -0.4921259842519685179, 0.3841425019411278674 ) ) ;
#1438 = CARTESIAN_POINT ( 'NONE',  ( -1.527714331928839098, 0.2380340132385416752, 0.05905511811023622659 ) ) ;
#1439 = CARTESIAN_POINT ( 'NONE',  ( -1.591501945092674841, 0.08600752902535288569, -0.08366141732283462196 ) ) ;
#1440 = VECTOR ( 'NONE', #5295, 39.37007874015748143 ) ;
#1441 = CARTESIAN_POINT ( 'NONE',  ( 0.2613315816342647868, -0.4881889763779528324, 0.03601011673569576993 ) ) ;
#1442 = CARTESIAN_POINT ( 'NONE',  ( 0.06767366483286080259, -0.2952755905511811330, 0.7209811753676967916 ) ) ;
#1443 = CIRCLE ( 'NONE', #5931, 0.003937007874015743640 ) ;
#1444 = EDGE_LOOP ( 'NONE', ( #205, #7671 ) ) ;
#1445 = PRODUCT_RELATED_PRODUCT_CATEGORY ( 'part', '', ( #309 ) ) ;
#1446 = EDGE_LOOP ( 'NONE', ( #3472, #11159, #6773, #2326 ) ) ;
#1447 = AXIS2_PLACEMENT_3D ( 'NONE', #15423, #4689, #5922 ) ;
#1448 = ORIENTED_EDGE ( 'NONE', *, *, #12770, .T. ) ;
#1449 = CARTESIAN_POINT ( 'NONE',  ( 2.025006518275150778E-17, -1.707404996040164512E-17, -0.1653543307086614012 ) ) ;
#1450 = FACE_OUTER_BOUND ( 'NONE', #3414, .T. ) ;
#1451 = DIRECTION ( 'NONE',  ( 0.000000000000000000, 0.000000000000000000, 1.000000000000000000 ) ) ;
#1452 = FACE_OUTER_BOUND ( 'NONE', #13767, .T. ) ;
#1453 = DIRECTION ( 'NONE',  ( -0.7484559191945134859, 0.5030755238499722282, -0.4321212264235259060 ) ) ;
#1454 = DIRECTION ( 'NONE',  ( 0.000000000000000000, 0.000000000000000000, -1.000000000000000000 ) ) ;
#1455 = CARTESIAN_POINT ( 'NONE',  ( -0.05270315828015968707, 0.1680450278838720446, 0.03205052537796105466 ) ) ;
#1456 = DIRECTION ( 'NONE',  ( -0.000000000000000000, -1.000000000000000000, -0.000000000000000000 ) ) ;
#1457 = FACE_OUTER_BOUND ( 'NONE', #6315, .T. ) ;
#1458 = CARTESIAN_POINT ( 'NONE',  ( -0.1552072824047653066, -0.09448818897637796532, -0.5870514566507987197 ) ) ;
#1459 = CIRCLE ( 'NONE', #4946, 0.003937007874015754916 ) ;
#1460 = CARTESIAN_POINT ( 'NONE',  ( 0.5418660417173575272, -0.4921259842519685179, 0.2355633981508976627 ) ) ;
#1461 = AXIS2_PLACEMENT_3D ( 'NONE', #5868, #15363, #9256 ) ;
#1462 = ORIENTED_EDGE ( 'NONE', *, *, #5234, .T. ) ;
#1463 = ADVANCED_FACE ( 'NONE', ( #4105 ), #2857, .F. ) ;
#1464 = ORIENTED_EDGE ( 'NONE', *, *, #9361, .T. ) ;
#1465 = ADVANCED_FACE ( 'NONE', ( #2945 ), #5641, .T. ) ;
#1466 = ORIENTED_EDGE ( 'NONE', *, *, #8268, .F. ) ;
#1467 = AXIS2_PLACEMENT_3D ( 'NONE', #1192, #9560, #12932 ) ;
#1468 = EDGE_CURVE ( 'NONE', #15072, #12817, #3016, .T. ) ;
#1469 = PLANE ( 'NONE',  #4835 ) ;
#1470 = CARTESIAN_POINT ( 'NONE',  ( -1.947525890741732768, -2.926847465874895526, -0.05663733393484523398 ) ) ;
#1471 = CARTESIAN_POINT ( 'NONE',  ( 0.1618514667033794374, -0.4881889763779528324, 0.2161887458866224576 ) ) ;
#1472 = VECTOR ( 'NONE', #7323, 39.37007874015748143 ) ;
#1473 = SPHERICAL_SURFACE ( 'NONE', #14206, 0.003937007874015747977 ) ;
#1474 = CARTESIAN_POINT ( 'NONE',  ( 0.1028896637646825596, -0.1023622047244094474, -0.2462933508111075365 ) ) ;
#1475 = DIRECTION ( 'NONE',  ( -0.000000000000000000, -1.000000000000000000, -0.000000000000000000 ) ) ;
#1476 = CARTESIAN_POINT ( 'NONE',  ( -0.2362204724409448231, -0.02638708502139245488, -0.03937007874015747977 ) ) ;
#1477 = CARTESIAN_POINT ( 'NONE',  ( 0.000000000000000000, 0.000000000000000000, 0.000000000000000000 ) ) ;
#1478 = CARTESIAN_POINT ( 'NONE',  ( 0.000000000000000000, 0.000000000000000000, 0.000000000000000000 ) ) ;
#1479 = CARTESIAN_POINT ( 'NONE',  ( -1.181102362204724310, 0.000000000000000000, -0.02559055118110236185 ) ) ;
#1480 = EDGE_LOOP ( 'NONE', ( #4243, #361, #13753, #4015 ) ) ;
#1481 = EDGE_CURVE ( 'NONE', #6389, #7333, #6762, .T. ) ;
#1482 = EDGE_LOOP ( 'NONE', ( #13423, #9079, #1781, #850 ) ) ;
#1483 = ORIENTED_EDGE ( 'NONE', *, *, #15195, .F. ) ;
#1484 = EDGE_CURVE ( 'NONE', #8826, #2247, #8802, .T. ) ;
#1485 = EDGE_LOOP ( 'NONE', ( #11055, #3153, #3263, #14893 ) ) ;
#1486 = ORIENTED_EDGE ( 'NONE', *, *, #3577, .F. ) ;
#1487 = CARTESIAN_POINT ( 'NONE',  ( -1.394658405437710913, -0.02432317279348940667, -0.06446726223640240894 ) ) ;
#1488 = ADVANCED_FACE ( 'NONE', ( #13033 ), #11633, .F. ) ;
#1489 = LINE ( 'NONE', #2734, #10112 ) ;
#1490 = DIRECTION ( 'NONE',  ( 1.000000000000000000, 0.000000000000000000, 0.000000000000000000 ) ) ;
#1491 = CARTESIAN_POINT ( 'NONE',  ( 0.7455328141524921737, 1.190944881889763884, 0.3622425942646917418 ) ) ;
#1492 = CARTESIAN_POINT ( 'NONE',  ( 0.4319503555479007328, -0.2952755905511811330, 0.1766496122645286049 ) ) ;
#1493 = CARTESIAN_POINT ( 'NONE',  ( -1.879798054437352262, -2.922014039083816073, -0.01138495494166368548 ) ) ;
#1494 = ORIENTED_EDGE ( 'NONE', *, *, #9429, .T. ) ;
#1495 = CARTESIAN_POINT ( 'NONE',  ( 0.5576140732134206024, -0.4881889763779528324, 0.2082870074805215910 ) ) ;
#1496 =( BOUNDED_CURVE ( )  B_SPLINE_CURVE ( 3, ( #4741, #10917, #43, #2693 ),
 .UNSPECIFIED., .F., .T. ) 
 B_SPLINE_CURVE_WITH_KNOTS ( ( 4, 4 ),
 ( 4.712388980384695003, 5.242505698889619481 ),
 .UNSPECIFIED. ) 
 CURVE ( )  GEOMETRIC_REPRESENTATION_ITEM ( )  RATIONAL_B_SPLINE_CURVE ( ( 1.000000000000000000, 0.9767181429391863512, 0.9767181429391863512, 1.000000000000000000 ) ) 
 REPRESENTATION_ITEM ( '' )  );
#1497 = CARTESIAN_POINT ( 'NONE',  ( -0.2647411304678976007, -0.09842519685039372024, 0.03404161279859290595 ) ) ;
#1498 = ORIENTED_EDGE ( 'NONE', *, *, #14031, .T. ) ;
#1499 = VERTEX_POINT ( 'NONE', #2062 ) ;
#1500 = ORIENTED_EDGE ( 'NONE', *, *, #14226, .F. ) ;
#1501 = EDGE_CURVE ( 'NONE', #8390, #15216, #4564, .T. ) ;
#1502 = SPHERICAL_SURFACE ( 'NONE', #3612, 0.003937007874015747977 ) ;
#1503 = DIRECTION ( 'NONE',  ( 1.000000000000000000, 0.000000000000000000, 0.000000000000000000 ) ) ;
#1504 = CYLINDRICAL_SURFACE ( 'NONE', #3473, 0.01968503937007877111 ) ;
#1505 = FACE_OUTER_BOUND ( 'NONE', #3880, .T. ) ;
#1506 = EDGE_LOOP ( 'NONE', ( #1005, #8758, #607, #6822 ) ) ;
#1507 = LINE ( 'NONE', #10984, #13420 ) ;
#1508 = EDGE_CURVE ( 'NONE', #9996, #3964, #11821, .T. ) ;
#1509 = CARTESIAN_POINT ( 'NONE',  ( -1.293236445124221312, 0.1355266887446167634, -0.05905511811023622659 ) ) ;
#1510 = CYLINDRICAL_SURFACE ( 'NONE', #14643, 0.03937007874015761855 ) ;
#1511 = LINE ( 'NONE', #9578, #12213 ) ;
#1512 = CARTESIAN_POINT ( 'NONE',  ( -0.1734555655881918346, -0.1023622047244094474, 0.1728816592724491952 ) ) ;
#1513 = EDGE_LOOP ( 'NONE', ( #4241, #2382, #3075, #751 ) ) ;
#1514 = VERTEX_POINT ( 'NONE', #6758 ) ;
#1515 = EDGE_LOOP ( 'NONE', ( #15107, #239, #15385, #13752 ) ) ;
#1516 = CARTESIAN_POINT ( 'NONE',  ( 1.181102362204724310, 4.044111181948214319E-16, 0.02952755905511811330 ) ) ;
#1517 = CARTESIAN_POINT ( 'NONE',  ( -0.05905511811023625435, 2.637795275590551825, -0.03937007874015747977 ) ) ;
#1518 = CARTESIAN_POINT ( 'NONE',  ( -0.05905511811012585655, -0.1023622047244094474, -0.5909884645248154600 ) ) ;
#1519 = CARTESIAN_POINT ( 'NONE',  ( -0.1724006475077544398, -0.4881889763779528324, 0.1768186671464649640 ) ) ;
#1520 = CARTESIAN_POINT ( 'NONE',  ( -0.1771653543307366296, 35.08612325493803041, -1.395267672073843279 ) ) ;
#1521 = CARTESIAN_POINT ( 'NONE',  ( 0.000000000000000000, 0.000000000000000000, 0.000000000000000000 ) ) ;
#1522 = FACE_OUTER_BOUND ( 'NONE', #4390, .T. ) ;
#1523 = CARTESIAN_POINT ( 'NONE',  ( 0.1618514667033794374, -0.4881889763779528324, 0.2122517380126066888 ) ) ;
#1524 = ADVANCED_FACE ( 'NONE', ( #902 ), #8097, .T. ) ;
#1525 = DIRECTION ( 'NONE',  ( 0.000000000000000000, 0.000000000000000000, -1.000000000000000000 ) ) ;
#1526 = CARTESIAN_POINT ( 'NONE',  ( 0.4307978335858664853, -0.09842519685039370636, 0.4318761856142889766 ) ) ;
#1527 = CARTESIAN_POINT ( 'NONE',  ( -0.7455328141524873997, 1.190944881889763884, 0.3622425942647021779 ) ) ;
#1528 = ORIENTED_EDGE ( 'NONE', *, *, #4288, .F. ) ;
#1529 = EDGE_LOOP ( 'NONE', ( #10287, #657, #4566, #2023 ) ) ;
#1530 = ORIENTED_EDGE ( 'NONE', *, *, #5773, .T. ) ;
#1531 = FACE_OUTER_BOUND ( 'NONE', #2276, .T. ) ;
#1532 = CARTESIAN_POINT ( 'NONE',  ( -1.940424138356921180, -2.944104218312575849, -0.04384797139731677618 ) ) ;
#1533 = DIRECTION ( 'NONE',  ( 1.000000000000000000, 0.000000000000000000, 0.000000000000000000 ) ) ;
#1534 = CARTESIAN_POINT ( 'NONE',  ( 0.5894146648244296127, -0.003937007874015747977, 0.1571437749735214717 ) ) ;
#1535 = CARTESIAN_POINT ( 'NONE',  ( 0.000000000000000000, 2.401574803149606918, 0.000000000000000000 ) ) ;
#1536 = DIRECTION ( 'NONE',  ( 0.4999999999999966693, 0.000000000000000000, 0.8660254037844405950 ) ) ;
#1537 = DIRECTION ( 'NONE',  ( 0.000000000000000000, -1.000000000000000000, 0.000000000000000000 ) ) ;
#1538 = EDGE_CURVE ( 'NONE', #2979, #6007, #12884, .T. ) ;
#1539 = CARTESIAN_POINT ( 'NONE',  ( -1.919185151238703479, -2.820797091852851768, 0.1478778761745188075 ) ) ;
#1540 = FACE_OUTER_BOUND ( 'NONE', #11225, .T. ) ;
#1541 = DIRECTION ( 'NONE',  ( 0.000000000000000000, 0.000000000000000000, -1.000000000000000000 ) ) ;
#1542 = VERTEX_POINT ( 'NONE', #5734 ) ;
#1543 = EDGE_CURVE ( 'NONE', #10323, #8667, #10374, .T. ) ;
#1544 = VERTEX_POINT ( 'NONE', #8191 ) ;
#1545 = ORIENTED_EDGE ( 'NONE', *, *, #10385, .F. ) ;
#1546 = VERTEX_POINT ( 'NONE', #8020 ) ;
#1547 = EDGE_LOOP ( 'NONE', ( #7478, #5200, #12563, #14223 ) ) ;
#1548 = DIRECTION ( 'NONE',  ( 0.8660254037844383745, 0.000000000000000000, 0.5000000000000004441 ) ) ;
#1549 = PRODUCT_DEFINITION_SHAPE ( 'NONE', 'NONE',  #15494 ) ;
#1550 = DIRECTION ( 'NONE',  ( 0.000000000000000000, 1.000000000000000000, 0.000000000000000000 ) ) ;
#1551 = DIRECTION ( 'NONE',  ( 0.8144815189573204606, -0.5801894994542525774, -1.283760644411384396E-16 ) ) ;
#1552 = EDGE_CURVE ( 'NONE', #8212, #8213, #2605, .T. ) ;
#1553 = CARTESIAN_POINT ( 'NONE',  ( -2.163017314575554906, -1.630597114118274238, 0.1033464566929130218 ) ) ;
#1554 = CARTESIAN_POINT ( 'NONE',  ( -1.187879871879865767, 0.3305938048772316673, 0.05905511811023621271 ) ) ;
#1555 = CARTESIAN_POINT ( 'NONE',  ( -1.902132589539931917, -2.937797416315981458, 0.06363563951555976927 ) ) ;
#1556 = ADVANCED_FACE ( 'NONE', ( #5507 ), #3490, .F. ) ;
#1557 = ORIENTED_EDGE ( 'NONE', *, *, #11175, .F. ) ;
#1558 = DIRECTION ( 'NONE',  ( 0.000000000000000000, 0.000000000000000000, 1.000000000000000000 ) ) ;
#1559 = CARTESIAN_POINT ( 'NONE',  ( -1.588286453767632000, 0.1240441066494159250, 0.03937007874189642903 ) ) ;
#1560 = DIRECTION ( 'NONE',  ( 0.000000000000000000, -0.000000000000000000, -1.000000000000000000 ) ) ;
#1561 = ORIENTED_EDGE ( 'NONE', *, *, #10820, .T. ) ;
#1562 = ADVANCED_FACE ( 'NONE', ( #2231 ), #10531, .F. ) ;
#1563 = ORIENTED_EDGE ( 'NONE', *, *, #6456, .T. ) ;
#1564 = ORIENTED_EDGE ( 'NONE', *, *, #702, .F. ) ;
#1565 = FACE_OUTER_BOUND ( 'NONE', #10973, .T. ) ;
#1566 =( BOUNDED_SURFACE ( )  B_SPLINE_SURFACE ( 3, 2, ( 
 ( #13244, #13476, #318 ),
 ( #8772, #7512, #14743 ),
 ( #3764, #2803, #1559 ),
 ( #2742, #13540, #8612 ) ),
 .UNSPECIFIED., .F., .F., .T. ) 
 B_SPLINE_SURFACE_WITH_KNOTS ( ( 4, 4 ),
 ( 3, 3 ),
 ( 4.182272261839050209, 4.712388980384689674 ),
 ( 0.000000000000000000, 1.000000000000000000 ),
 .UNSPECIFIED. ) 
 GEOMETRIC_REPRESENTATION_ITEM ( )  RATIONAL_B_SPLINE_SURFACE ( (
 ( 1.000000000000000000, 0.7111298678012015761, 1.000000000000000000),
 ( 1.000000000000000000, 0.7099209393060977868, 1.000000000000000000),
 ( 1.000000000000000000, 0.7085172298915587419, 1.000000000000000000),
 ( 1.000000000000000000, 0.7071067811865475727, 1.000000000000000000) ) ) 
 REPRESENTATION_ITEM ( '' )  SURFACE ( )  );
#1567 = FACE_OUTER_BOUND ( 'NONE', #8723, .T. ) ;
#1568 = CARTESIAN_POINT ( 'NONE',  ( -2.163017314575554462, -1.630597114118274238, -0.08366141732283423338 ) ) ;
#1569 = CARTESIAN_POINT ( 'NONE',  ( -0.06327586242532841354, -0.1861954285973654311, -0.03830155300069465474 ) ) ;
#1570 = EDGE_CURVE ( 'NONE', #8667, #8301, #11791, .T. ) ;
#1571 = ORIENTED_EDGE ( 'NONE', *, *, #5696, .F. ) ;
#1572 = CARTESIAN_POINT ( 'NONE',  ( -2.077963565069627982, -2.158389492283137479, 0.09850863663452619212 ) ) ;
#1573 = DIRECTION ( 'NONE',  ( 0.000000000000000000, 0.000000000000000000, 1.000000000000000000 ) ) ;
#1574 = CIRCLE ( 'NONE', #6567, 0.007874015748031449116 ) ;
#1575 = CIRCLE ( 'NONE', #10326, 0.003937007874015750579 ) ;
#1576 = CARTESIAN_POINT ( 'NONE',  ( -1.234181327013985197, 0.1355266887446167634, -0.05905511811023622659 ) ) ;
#1577 = AXIS2_PLACEMENT_3D ( 'NONE', #8678, #2488, #13227 ) ;
#1578 = ADVANCED_FACE ( 'NONE', ( #1055 ), #4420, .F. ) ;
#1579 = CARTESIAN_POINT ( 'NONE',  ( -1.419615703680148000, -0.01226548409420231273, -0.07874015748031495954 ) ) ;
#1580 = CIRCLE ( 'NONE', #8334, 0.2165354330708662012 ) ;
#1581 = EDGE_CURVE ( 'NONE', #12382, #11226, #11954, .T. ) ;
#1582 = ORIENTED_EDGE ( 'NONE', *, *, #8272, .F. ) ;
#1583 = ORIENTED_EDGE ( 'NONE', *, *, #6988, .T. ) ;
#1584 = ORIENTED_EDGE ( 'NONE', *, *, #11099, .T. ) ;
#1585 = EDGE_CURVE ( 'NONE', #984, #9393, #12803, .T. ) ;
#1586 = DIRECTION ( 'NONE',  ( 0.000000000000000000, 0.000000000000000000, -1.000000000000000000 ) ) ;
#1587 = CARTESIAN_POINT ( 'NONE',  ( 0.7796283024904624437, 1.190944881889763884, 0.3819276336347702805 ) ) ;
#1588 = CIRCLE ( 'NONE', #5578, 0.5905511811023621549 ) ;
#1589 = VECTOR ( 'NONE', #8066, 39.37007874015748143 ) ;
#1590 = DIRECTION ( 'NONE',  ( -0.000000000000000000, -1.000000000000000000, -0.000000000000000000 ) ) ;
#1591 = DIRECTION ( 'NONE',  ( -1.000000000000000000, -0.000000000000000000, -0.000000000000000000 ) ) ;
#1592 = CIRCLE ( 'NONE', #107, 0.007874015748031499423 ) ;
#1593 =( CONVERSION_BASED_UNIT ( 'INCH', #7771 ) LENGTH_UNIT ( ) NAMED_UNIT ( #6742 ) );
#1594 = CARTESIAN_POINT ( 'NONE',  ( -1.992382107315057160, -2.749515453455444014, -0.1756903148397123138 ) ) ;
#1595 = DIRECTION ( 'NONE',  ( -0.000000000000000000, -1.000000000000000000, -0.000000000000000000 ) ) ;
#1596 = DIRECTION ( 'NONE',  ( 0.000000000000000000, -1.000000000000000000, 0.000000000000000000 ) ) ;
#1597 = CARTESIAN_POINT ( 'NONE',  ( 0.03357817649489055339, -0.2952755905511811330, 0.7012961359976183084 ) ) ;
#1598 = DIRECTION ( 'NONE',  ( 0.000000000000000000, 0.000000000000000000, 1.000000000000000000 ) ) ;
#1599 = VERTEX_POINT ( 'NONE', #14926 ) ;
#1600 = ADVANCED_FACE ( 'NONE', ( #10445 ), #8436, .F. ) ;
#1601 = AXIS2_PLACEMENT_3D ( 'NONE', #2236, #5740, #992 ) ;
#1602 = CIRCLE ( 'NONE', #7591, 0.7086614173228346081 ) ;
#1603 = ORIENTED_EDGE ( 'NONE', *, *, #8939, .F. ) ;
#1604 = VECTOR ( 'NONE', #8856, 39.37007874015748143 ) ;
#1605 = CARTESIAN_POINT ( 'NONE',  ( -0.4307978335858689833, -0.003937007874015747977, 0.4279391777402706265 ) ) ;
#1606 = AXIS2_PLACEMENT_3D ( 'NONE', #9961, #1648, #6406 ) ;
#1607 = ORIENTED_EDGE ( 'NONE', *, *, #13477, .F. ) ;
#1608 = TOROIDAL_SURFACE ( 'NONE', #8118, 0.04330708661417328326, 0.003937007874015747977 ) ;
#1609 = ORIENTED_EDGE ( 'NONE', *, *, #2027, .F. ) ;
#1610 = EDGE_CURVE ( 'NONE', #4124, #6576, #13195, .T. ) ;
#1611 = DIRECTION ( 'NONE',  ( 0.4999999999999996114, 0.000000000000000000, 0.8660254037844389297 ) ) ;
#1612 = CARTESIAN_POINT ( 'NONE',  ( -1.940983278890547004, -2.905281415726287619, 0.1177841364776334443 ) ) ;
#1613 = CIRCLE ( 'NONE', #11882, 0.003937007874015758385 ) ;
#1614 = AXIS2_PLACEMENT_3D ( 'NONE', #7716, #12504, #10148 ) ;
#1615 = TOROIDAL_SURFACE ( 'NONE', #3622, 0.5590551181102362266, 0.007874015748031495954 ) ;
#1616 = CARTESIAN_POINT ( 'NONE',  ( 0.000000000000000000, 0.000000000000000000, 0.000000000000000000 ) ) ;
#1617 = CIRCLE ( 'NONE', #10371, 0.1574803149606299191 ) ;
#1618 = TOROIDAL_SURFACE ( 'NONE', #11632, 0.04330708661417328326, 0.003937007874015747977 ) ;
#1619 = CARTESIAN_POINT ( 'NONE',  ( -2.003351654124630343, -2.780426454911686829, -0.1578453099020075412 ) ) ;
#1620 = CARTESIAN_POINT ( 'NONE',  ( 1.181102362204724310, 4.044111181948214319E-16, 0.02559055118110236185 ) ) ;
#1621 = CIRCLE ( 'NONE', #10876, 0.003937007874015758385 ) ;
#1622 = DIRECTION ( 'NONE',  ( -0.08188191145426276796, 0.000000000000000000, 0.9966420383350264034 ) ) ;
#1623 = B_SPLINE_CURVE_WITH_KNOTS ( 'NONE', 3,
 ( #499, #1669, #12040, #14822 ),
 .UNSPECIFIED., .F., .F.,
 ( 4, 4 ),
 ( 0.000000000000000000, 2.119993237936282563E-05 ),
 .UNSPECIFIED. ) ;
#1624 = CARTESIAN_POINT ( 'NONE',  ( -1.417802900492933782, -0.04287136159519136513, 0.08366141732283458032 ) ) ;
#1625 = CYLINDRICAL_SURFACE ( 'NONE', #6824, 0.2106299212598417292 ) ;
#1626 = DIRECTION ( 'NONE',  ( 0.5000000000000003331, 0.000000000000000000, -0.8660254037844387076 ) ) ;
#1627 = VERTEX_POINT ( 'NONE', #10358 ) ;
#1628 = ORIENTED_EDGE ( 'NONE', *, *, #5394, .F. ) ;
#1629 = VECTOR ( 'NONE', #12264, 39.37007874015748143 ) ;
#1630 = ORIENTED_EDGE ( 'NONE', *, *, #2426, .F. ) ;
#1631 = AXIS2_PLACEMENT_3D ( 'NONE', #1993, #2225, #13029 ) ;
#1632 = CIRCLE ( 'NONE', #1387, 0.04330708661417331101 ) ;
#1633 = ORIENTED_EDGE ( 'NONE', *, *, #53, .T. ) ;
#1634 = ORIENTED_EDGE ( 'NONE', *, *, #4954, .T. ) ;
#1635 = VECTOR ( 'NONE', #6238, 39.37007874015748143 ) ;
#1636 = DIRECTION ( 'NONE',  ( 0.000000000000000000, 0.000000000000000000, -1.000000000000000000 ) ) ;
#1637 = CARTESIAN_POINT ( 'NONE',  ( 0.1062992125984796865, -0.09448818897637796532, -0.5909884645248143498 ) ) ;
#1638 = CARTESIAN_POINT ( 'NONE',  ( 0.5433070866142283295, -0.1023622047244094474, 0.2409414509217496780 ) ) ;
#1639 = DIRECTION ( 'NONE',  ( 0.4999999999999966693, 0.000000000000000000, 0.8660254037844405950 ) ) ;
#1640 = CARTESIAN_POINT ( 'NONE',  ( 1.904470415996868375E-17, -0.4921259842519685179, 0.1535433070866141780 ) ) ;
#1641 = FACE_OUTER_BOUND ( 'NONE', #1039, .T. ) ;
#1642 = CIRCLE ( 'NONE', #8139, 0.6692913385826770867 ) ;
#1643 = LINE ( 'NONE', #2798, #11183 ) ;
#1644 = AXIS2_PLACEMENT_3D ( 'NONE', #497, #14819, #5241 ) ;
#1645 = CARTESIAN_POINT ( 'NONE',  ( -1.890104583037259589, -2.896615591685024249, 0.08668355014530308711 ) ) ;
#1646 = EDGE_LOOP ( 'NONE', ( #5437, #10259, #3434, #3376 ) ) ;
#1647 = DIRECTION ( 'NONE',  ( 0.000000000000000000, 0.000000000000000000, -1.000000000000000000 ) ) ;
#1648 = DIRECTION ( 'NONE',  ( 0.5984233124757313282, 0.8011800915434514891, 0.000000000000000000 ) ) ;
#1649 = CIRCLE ( 'NONE', #163, 0.5511811023622046335 ) ;
#1650 = DIRECTION ( 'NONE',  ( 0.000000000000000000, -1.000000000000000000, 0.000000000000000000 ) ) ;
#1651 = ORIENTED_EDGE ( 'NONE', *, *, #5556, .F. ) ;
#1652 = ORIENTED_EDGE ( 'NONE', *, *, #2355, .F. ) ;
#1653 = ADVANCED_FACE ( 'NONE', ( #13746 ), #1989, .T. ) ;
#1654 = ORIENTED_EDGE ( 'NONE', *, *, #1746, .T. ) ;
#1655 = VECTOR ( 'NONE', #7555, 39.37007874015748143 ) ;
#1656 = ADVANCED_FACE ( 'NONE', ( #6750, #13975 ), #2050, .F. ) ;
#1657 = VECTOR ( 'NONE', #10481, 39.37007874015748143 ) ;
#1658 = CIRCLE ( 'NONE', #11418, 0.007874015748031449116 ) ;
#1659 = EDGE_CURVE ( 'NONE', #11443, #4974, #9690, .T. ) ;
#1660 = DIRECTION ( 'NONE',  ( 0.000000000000000000, 0.000000000000000000, 1.000000000000000000 ) ) ;
#1661 = CARTESIAN_POINT ( 'NONE',  ( -0.08199009355444111802, 0.06963377358818916008, -0.01990370102563917068 ) ) ;
#1662 = CARTESIAN_POINT ( 'NONE',  ( -0.07874015748031520934, 1.062385330869439640E-16, -0.01968503937007873988 ) ) ;
#1663 = DIRECTION ( 'NONE',  ( 0.5000000000000036637, -0.000000000000000000, 0.8660254037844364872 ) ) ;
#1664 = ORIENTED_EDGE ( 'NONE', *, *, #2711, .T. ) ;
#1665 = DIRECTION ( 'NONE',  ( -0.5000000000000003331, -0.000000000000000000, 0.8660254037844387076 ) ) ;
#1666 = CARTESIAN_POINT ( 'NONE',  ( -1.596030944582063960, 0.1136756404979306911, -0.04477369844321314740 ) ) ;
#1667 = CARTESIAN_POINT ( 'NONE',  ( 0.9851651268172137987, -1.725292181286280480, 0.08366141732283420562 ) ) ;
#1668 = AXIS2_PLACEMENT_3D ( 'NONE', #1527, #4899, #3961 ) ;
#1669 = CARTESIAN_POINT ( 'NONE',  ( -0.5447670804912987386, 1.043292445042268257, 0.2463304438913610228 ) ) ;
#1670 = DIRECTION ( 'NONE',  ( 0.000000000000000000, 0.000000000000000000, 1.000000000000000000 ) ) ;
#1671 = CIRCLE ( 'NONE', #186, 0.5905511811023621549 ) ;
#1672 = VERTEX_POINT ( 'NONE', #10219 ) ;
#1673 = EDGE_CURVE ( 'NONE', #2506, #9877, #6922, .T. ) ;
#1674 = ORIENTED_EDGE ( 'NONE', *, *, #13331, .T. ) ;
#1675 = EDGE_CURVE ( 'NONE', #7280, #9631, #15001, .T. ) ;
#1676 = ORIENTED_EDGE ( 'NONE', *, *, #1937, .F. ) ;
#1677 = CARTESIAN_POINT ( 'NONE',  ( -0.5860051159906336515, -0.003937007874015747977, 0.1591122789105256785 ) ) ;
#1678 = FACE_OUTER_BOUND ( 'NONE', #11676, .T. ) ;
#1679 = AXIS2_PLACEMENT_3D ( 'NONE', #9203, #13264, #2523 ) ;
#1680 = EDGE_CURVE ( 'NONE', #8643, #5718, #2923, .T. ) ;
#1681 = CARTESIAN_POINT ( 'NONE',  ( -1.961142902483386852, -2.698831051917248480, 0.1691401727068858885 ) ) ;
#1682 = DIRECTION ( 'NONE',  ( -0.8660254037844395958, 0.000000000000000000, 0.4999999999999982236 ) ) ;
#1683 = AXIS2_PLACEMENT_3D ( 'NONE', #14080, #939, #3352 ) ;
#1684 = CARTESIAN_POINT ( 'NONE',  ( -1.987685136288601218, -2.764754373406230314, -0.1771653543307125100 ) ) ;
#1685 = FACE_OUTER_BOUND ( 'NONE', #8518, .T. ) ;
#1686 = DIRECTION ( 'NONE',  ( 0.000000000000000000, 1.000000000000000000, 0.000000000000000000 ) ) ;
#1687 = DIRECTION ( 'NONE',  ( 0.000000000000000000, -1.000000000000000000, -0.000000000000000000 ) ) ;
#1688 = CIRCLE ( 'NONE', #5920, 0.03937007874015751446 ) ;
#1689 = EDGE_LOOP ( 'NONE', ( #3630, #60, #946, #5736 ) ) ;
#1690 = AXIS2_PLACEMENT_3D ( 'NONE', #2211, #5786, #4396 ) ;
#1691 = ORIENTED_EDGE ( 'NONE', *, *, #15456, .T. ) ;
#1692 = DIRECTION ( 'NONE',  ( 0.000000000000000000, 0.000000000000000000, 1.000000000000000000 ) ) ;
#1693 = ORIENTED_EDGE ( 'NONE', *, *, #8707, .T. ) ;
#1694 = AXIS2_PLACEMENT_3D ( 'NONE', #599, #5210, #1774 ) ;
#1695 = VERTEX_POINT ( 'NONE', #6585 ) ;
#1696 = DIRECTION ( 'NONE',  ( 0.4999999999999918954, -0.000000000000000000, -0.8660254037844431485 ) ) ;
#1697 = CARTESIAN_POINT ( 'NONE',  ( -1.944063115746497372, -2.896559852577519134, 0.1269213948424093574 ) ) ;
#1698 = EDGE_CURVE ( 'NONE', #7635, #532, #11684, .T. ) ;
#1699 = AXIS2_PLACEMENT_3D ( 'NONE', #819, #5744, #4339 ) ;
#1700 = DIRECTION ( 'NONE',  ( 0.5000000000000035527, 0.000000000000000000, -0.8660254037844365982 ) ) ;
#1701 =( REPRESENTATION_RELATIONSHIP ('NONE','NONE', #8904, #7785 ) REPRESENTATION_RELATIONSHIP_WITH_TRANSFORMATION ( #4408 )SHAPE_REPRESENTATION_RELATIONSHIP( ) );
#1702 = CARTESIAN_POINT ( 'NONE',  ( -2.007605986780809815, -2.768314085474279373, -0.1776672152077323208 ) ) ;
#1703 = CARTESIAN_POINT ( 'NONE',  ( 0.000000000000000000, 0.5984251968503937480, 0.000000000000000000 ) ) ;
#1704 = TOROIDAL_SURFACE ( 'NONE', #14975, 0.04330708661417328326, 0.003937007874015747977 ) ;
#1705 = PLANE ( 'NONE',  #2645 ) ;
#1706 = CARTESIAN_POINT ( 'NONE',  ( -0.01545036047008872468, -0.1795454119435216378, -8.867015126428109484E-14 ) ) ;
#1707 = EDGE_CURVE ( 'NONE', #1942, #532, #189, .T. ) ;
#1708 = DIRECTION ( 'NONE',  ( 0.000000000000000000, 0.000000000000000000, 1.000000000000000000 ) ) ;
#1709 = DIRECTION ( 'NONE',  ( -0.000000000000000000, -1.000000000000000000, -0.000000000000000000 ) ) ;
#1710 = EDGE_LOOP ( 'NONE', ( #7050, #11774, #11724, #13595 ) ) ;
#1711 = ORIENTED_EDGE ( 'NONE', *, *, #12080, .T. ) ;
#1712 = VECTOR ( 'NONE', #2678, 39.37007874015748143 ) ;
#1713 = ORIENTED_EDGE ( 'NONE', *, *, #10319, .F. ) ;
#1714 = ORIENTED_EDGE ( 'NONE', *, *, #8843, .F. ) ;
#1715 = ORIENTED_EDGE ( 'NONE', *, *, #14031, .F. ) ;
#1716 = CIRCLE ( 'NONE', #14472, 0.01968503937007873988 ) ;
#1717 = DIRECTION ( 'NONE',  ( 0.5000000000000000000, 0.000000000000000000, -0.8660254037844385966 ) ) ;
#1718 = CARTESIAN_POINT ( 'NONE',  ( -0.5084014747882513729, -0.09842519685039370636, 0.2935257283253980831 ) ) ;
#1719 = CARTESIAN_POINT ( 'NONE',  ( 0.06692913385832209572, -0.4881889763779528324, -0.2377126739437404879 ) ) ;
#1720 = CARTESIAN_POINT ( 'NONE',  ( -0.1968503937007873295, -0.02638708502139245141, 0.03937007874015747977 ) ) ;
#1721 = CARTESIAN_POINT ( 'NONE',  ( -0.5595825771504281398, -0.4881889763779528324, 0.2048774586467239645 ) ) ;
#1722 = DIRECTION ( 'NONE',  ( 0.000000000000000000, -1.000000000000000000, 0.000000000000000000 ) ) ;
#1723 = DIRECTION ( 'NONE',  ( -0.000000000000000000, -1.000000000000000000, -0.000000000000000000 ) ) ;
#1725 = CIRCLE ( 'NONE', #9979, 0.05905511811023625435 ) ;
#1724 = SPHERICAL_SURFACE ( 'NONE', #9947, 0.003937007874015747977 ) ;
#1726 = CARTESIAN_POINT ( 'NONE',  ( -1.878738707309701272, -2.924867600962848702, -0.09124266643724603110 ) ) ;
#1727 = ORIENTED_EDGE ( 'NONE', *, *, #428, .F. ) ;
#1728 = DIRECTION ( 'NONE',  ( 0.000000000000000000, 0.000000000000000000, -1.000000000000000000 ) ) ;
#1729 = DIRECTION ( 'NONE',  ( 0.000000000000000000, 0.000000000000000000, 1.000000000000000000 ) ) ;
#1730 = VERTEX_POINT ( 'NONE', #4409 ) ;
#1731 = VERTEX_POINT ( 'NONE', #11473 ) ;
#1732 = ORIENTED_EDGE ( 'NONE', *, *, #8232, .T. ) ;
#1733 = DIRECTION ( 'NONE',  ( -1.504632769052539669E-28, -8.673617379884051249E-15, 1.000000000000000000 ) ) ;
#1734 = DIRECTION ( 'NONE',  ( 1.000000000000000000, -0.000000000000000000, 1.224646799147353207E-16 ) ) ;
#1735 = CARTESIAN_POINT ( 'NONE',  ( 0.000000000000000000, 1.425196850393700920, -0.6614173228346456046 ) ) ;
#1736 = CARTESIAN_POINT ( 'NONE',  ( 0.000000000000000000, 0.5511811023622046335, 0.000000000000000000 ) ) ;
#1737 = DIRECTION ( 'NONE',  ( 2.309263891220325920E-14, 0.000000000000000000, -1.000000000000000000 ) ) ;
#1738 = ORIENTED_EDGE ( 'NONE', *, *, #5192, .F. ) ;
#1739 = ADVANCED_FACE ( 'NONE', ( #9195 ), #2673, .F. ) ;
#1740 = CYLINDRICAL_SURFACE ( 'NONE', #4919, 0.003937007874015735834 ) ;
#1741 = DIRECTION ( 'NONE',  ( -1.000000000000000000, 0.000000000000000000, 0.000000000000000000 ) ) ;
#1742 = CARTESIAN_POINT ( 'NONE',  ( 0.05905511811023622659, 1.043307086614173373, -0.5511811023622047445 ) ) ;
#1743 = EDGE_CURVE ( 'NONE', #4061, #4031, #13436, .T. ) ;
#1744 = DIRECTION ( 'NONE',  ( 0.000000000000000000, 0.000000000000000000, 1.000000000000000000 ) ) ;
#1745 = ORIENTED_EDGE ( 'NONE', *, *, #9638, .F. ) ;
#1746 = EDGE_CURVE ( 'NONE', #12957, #11239, #3028, .T. ) ;
#1747 = ORIENTED_EDGE ( 'NONE', *, *, #5493, .T. ) ;
#1748 = DIRECTION ( 'NONE',  ( 0.8660254037844385966, 0.000000000000000000, -0.4999999999999998890 ) ) ;
#1749 = FACE_OUTER_BOUND ( 'NONE', #3031, .T. ) ;
#1750 = CARTESIAN_POINT ( 'NONE',  ( -0.08151194962748890827, 0.1637246173173402264, -0.05905511811023622659 ) ) ;
#1751 = CARTESIAN_POINT ( 'NONE',  ( -0.05114323250695503725, 0.000000000000000000, -0.08858267716535432601 ) ) ;
#1752 = APPLICATION_PROTOCOL_DEFINITION ( 'draft international standard', 'automotive_design', 1998, #8399 ) ;
#1753 = DIRECTION ( 'NONE',  ( 0.000000000000000000, -1.000000000000000000, 0.000000000000000000 ) ) ;
#1754 = CARTESIAN_POINT ( 'NONE',  ( -1.990041936606229189, -2.757150128560895475, -0.1766817015956954062 ) ) ;
#1755 = ADVANCED_FACE ( 'NONE', ( #12494 ), #9459, .T. ) ;
#1756 = DIRECTION ( 'NONE',  ( 0.8660254037844459241, 0.000000000000000000, 0.4999999999999873990 ) ) ;
#1757 = CARTESIAN_POINT ( 'NONE',  ( -0.4572203724260467950, -0.4921259842519685179, 0.3821739980041202744 ) ) ;
#1758 = ADVANCED_FACE ( 'NONE', ( #5497 ), #13889, .F. ) ;
#1759 = FACE_OUTER_BOUND ( 'NONE', #10317, .T. ) ;
#1760 = EDGE_CURVE ( 'NONE', #6534, #10712, #8315, .T. ) ;
#1761 = DIRECTION ( 'NONE',  ( -1.445602896647339903E-16, -0.000000000000000000, 1.000000000000000000 ) ) ;
#1762 = ORIENTED_EDGE ( 'NONE', *, *, #2654, .T. ) ;
#1763 = ORIENTED_EDGE ( 'NONE', *, *, #8788, .T. ) ;
#1764 = EDGE_CURVE ( 'NONE', #5035, #11956, #7944, .T. ) ;
#1765 = ORIENTED_EDGE ( 'NONE', *, *, #13389, .F. ) ;
#1766 = ORIENTED_EDGE ( 'NONE', *, *, #11796, .T. ) ;
#1767 = CARTESIAN_POINT ( 'NONE',  ( 0.5398975377803496567, -0.09842519685039372024, 0.2389729469846946508 ) ) ;
#1768 = CARTESIAN_POINT ( 'NONE',  ( -1.993480072126341041, -2.602359853078048513, -0.1374116847797290930 ) ) ;
#1769 = CARTESIAN_POINT ( 'NONE',  ( -1.309055118110236116, 0.000000000000000000, -0.02559055118110236185 ) ) ;
#1770 = CARTESIAN_POINT ( 'NONE',  ( -1.965394281685034050, -2.834131647928828546, -0.1664892934202782671 ) ) ;
#1771 = CARTESIAN_POINT ( 'NONE',  ( 0.2647411304680618027, -0.1023622047244094474, 0.03404161279868787859 ) ) ;
#1772 = DIRECTION ( 'NONE',  ( 0.000000000000000000, 0.000000000000000000, -1.000000000000000000 ) ) ;
#1773 = EDGE_CURVE ( 'NONE', #8290, #3157, #14124, .T. ) ;
#1774 = DIRECTION ( 'NONE',  ( -0.8660254037844390407, 0.000000000000000000, 0.4999999999999994449 ) ) ;
#1775 = FACE_OUTER_BOUND ( 'NONE', #1513, .T. ) ;
#1776 = CARTESIAN_POINT ( 'NONE',  ( -2.090210618530727871, -1.821590950714383261, -0.1053165596881613930 ) ) ;
#1777 = ORIENTED_EDGE ( 'NONE', *, *, #6701, .F. ) ;
#1778 = EDGE_CURVE ( 'NONE', #7138, #7284, #14200, .T. ) ;
#1779 = ORIENTED_EDGE ( 'NONE', *, *, #1964, .T. ) ;
#1780 = ADVANCED_FACE ( 'NONE', ( #3626 ), #6027, .F. ) ;
#1781 = ORIENTED_EDGE ( 'NONE', *, *, #13152, .T. ) ;
#1782 = ORIENTED_EDGE ( 'NONE', *, *, #991, .F. ) ;
#1783 = ORIENTED_EDGE ( 'NONE', *, *, #12115, .F. ) ;
#1784 = CARTESIAN_POINT ( 'NONE',  ( -1.419615703584982569, -0.01226548416199267633, -0.07606650080514479328 ) ) ;
#1785 = EDGE_CURVE ( 'NONE', #6404, #9753, #8402, .T. ) ;
#1786 = DIRECTION ( 'NONE',  ( 0.000000000000000000, 1.000000000000000000, 0.000000000000000000 ) ) ;
#1787 = CARTESIAN_POINT ( 'NONE',  ( -0.05905511811023622659, 1.338582677165354395, -0.8267716535433070613 ) ) ;
#1788 = LINE ( 'NONE', #5525, #4435 ) ;
#1789 = LINE ( 'NONE', #10248, #611 ) ;
#1790 = CARTESIAN_POINT ( 'NONE',  ( 0.000000000000000000, 1.614173228346457156, 0.5590551181102362266 ) ) ;
#1791 = DIRECTION ( 'NONE',  ( 1.000000000000000000, 0.000000000000000000, 0.000000000000000000 ) ) ;
#1792 = CARTESIAN_POINT ( 'NONE',  ( -0.5418660417173573052, -0.09842519685039370636, 0.2355633981508970798 ) ) ;
#1793 = CARTESIAN_POINT ( 'NONE',  ( 0.05905511811023622659, 1.043263280880422528, -0.5946706712680680518 ) ) ;
#1794 = ORIENTED_EDGE ( 'NONE', *, *, #12680, .F. ) ;
#1795 = DIRECTION ( 'NONE',  ( -0.4999999999999995004, -0.000000000000000000, -0.8660254037844390407 ) ) ;
#1796 = CARTESIAN_POINT ( 'NONE',  ( 8.196454954923229282E-17, 0.3622047244094487306, 0.6692913385826770867 ) ) ;
#1797 = VERTEX_POINT ( 'NONE', #5964 ) ;
#1798 = ORIENTED_EDGE ( 'NONE', *, *, #2623, .F. ) ;
#1799 = EDGE_LOOP ( 'NONE', ( #10229, #6759, #4858, #1287 ) ) ;
#1800 = EDGE_CURVE ( 'NONE', #14240, #8264, #12703, .T. ) ;
#1801 = DIRECTION ( 'NONE',  ( -1.000000000000000000, 0.000000000000000000, -3.075191616504340279E-15 ) ) ;
#1802 = DIRECTION ( 'NONE',  ( 0.8660254037844385966, 0.000000000000000000, -0.4999999999999998890 ) ) ;
#1803 = DIRECTION ( 'NONE',  ( 0.000000000000000000, 2.212657494868377674E-16, 1.000000000000000000 ) ) ;
#1804 = CARTESIAN_POINT ( 'NONE',  ( -0.07635964791965738074, -0.1878198040935885327, -0.03937007874015747977 ) ) ;
#1805 = ORIENTED_EDGE ( 'NONE', *, *, #14342, .F. ) ;
#1806 = LINE ( 'NONE', #3933, #926 ) ;
#1807 = DIRECTION ( 'NONE',  ( -0.8144815189573203495, 0.5801894994542524664, -0.000000000000000000 ) ) ;
#1808 = CARTESIAN_POINT ( 'NONE',  ( -0.004461712539986224628, -0.1607679992104108779, 0.007865172455356563355 ) ) ;
#1809 = FACE_OUTER_BOUND ( 'NONE', #6119, .T. ) ;
#1810 = VERTEX_POINT ( 'NONE', #11784 ) ;
#1811 = ORIENTED_EDGE ( 'NONE', *, *, #8765, .F. ) ;
#1812 = ORIENTED_EDGE ( 'NONE', *, *, #5688, .F. ) ;
#1813 = ORIENTED_EDGE ( 'NONE', *, *, #5250, .F. ) ;
#1814 = FACE_OUTER_BOUND ( 'NONE', #4208, .T. ) ;
#1815 = CARTESIAN_POINT ( 'NONE',  ( -2.100501784635051550, -1.630597114118274460, 0.08366141732283423338 ) ) ;
#1816 = CARTESIAN_POINT ( 'NONE',  ( -0.06144837730693395589, 0.1461156186057537831, -0.05762996311186197040 ) ) ;
#1817 = FACE_OUTER_BOUND ( 'NONE', #11527, .T. ) ;
#1818 = CARTESIAN_POINT ( 'NONE',  ( 2.419703784132994590E-19, 0.07093549527207483607, -0.07900545476875228679 ) ) ;
#1819 = CIRCLE ( 'NONE', #826, 0.04330708661417328326 ) ;
#1820 = DIRECTION ( 'NONE',  ( -1.000000000000000000, -0.000000000000000000, -3.476578583725179813E-16 ) ) ;
#1821 = ORIENTED_EDGE ( 'NONE', *, *, #1707, .T. ) ;
#1822 = LINE ( 'NONE', #438, #7406 ) ;
#1823 = CIRCLE ( 'NONE', #14629, 0.05905511811023620578 ) ;
#1824 = ADVANCED_FACE ( 'NONE', ( #13186 ), #2220, .T. ) ;
#1825 = DIRECTION ( 'NONE',  ( -0.000000000000000000, 1.000000000000000000, 0.000000000000000000 ) ) ;
#1826 = AXIS2_PLACEMENT_3D ( 'NONE', #1491, #2499, #6239 ) ;
#1827 = CARTESIAN_POINT ( 'NONE',  ( 0.5615510810874363434, -0.09842519685039370636, 0.2014679098129276424 ) ) ;
#1828 = CARTESIAN_POINT ( 'NONE',  ( 0.06299212598430634080, -0.4881889763779528324, -0.2366577558633030653 ) ) ;
#1829 = ORIENTED_EDGE ( 'NONE', *, *, #4344, .F. ) ;
#1830 = EDGE_LOOP ( 'NONE', ( #3385, #4258 ) ) ;
#1831 = CARTESIAN_POINT ( 'NONE',  ( 0.000000000000000000, -0.4921259842519685179, 0.000000000000000000 ) ) ;
#1832 = VERTEX_POINT ( 'NONE', #30 ) ;
#1833 = CIRCLE ( 'NONE', #2832, 0.2106299212598415904 ) ;
#1834 = ORIENTED_EDGE ( 'NONE', *, *, #6073, .F. ) ;
#1835 = AXIS2_PLACEMENT_3D ( 'NONE', #4970, #13213, #7250 ) ;
#1836 = TOROIDAL_SURFACE ( 'NONE', #10600, 0.5826771653543306728, 0.007874015748031495954 ) ;
#1837 = ADVANCED_FACE ( 'NONE', ( #13025 ), #12870, .T. ) ;
#1838 = CARTESIAN_POINT ( 'NONE',  ( -0.09061599198715356018, 0.06736074103232447818, -0.007444810018878696839 ) ) ;
#1839 = DIRECTION ( 'NONE',  ( -0.000000000000000000, -1.000000000000000000, -0.000000000000000000 ) ) ;
#1840 = B_SPLINE_CURVE_WITH_KNOTS ( 'NONE', 3,
 ( #7392, #6441, #5185, #3869 ),
 .UNSPECIFIED., .F., .F.,
 ( 4, 4 ),
 ( 2.006738551125145802E-07, 0.0009905856238791850652 ),
 .UNSPECIFIED. ) ;
#1841 = LINE ( 'NONE', #1928, #8964 ) ;
#1842 = ADVANCED_FACE ( 'NONE', ( #10593 ), #14209, .T. ) ;
#1843 = CARTESIAN_POINT ( 'NONE',  ( 0.2613315816342647868, -0.4921259842519685179, 0.03601011673569576993 ) ) ;
#1844 = DIRECTION ( 'NONE',  ( 0.000000000000000000, 0.000000000000000000, 1.000000000000000000 ) ) ;
#1845 = AXIS2_PLACEMENT_3D ( 'NONE', #10153, #13513, #11403 ) ;
#1846 = CIRCLE ( 'NONE', #10607, 0.003937007874015721089 ) ;
#1847 = CARTESIAN_POINT ( 'NONE',  ( 0.000000000000000000, 2.165354330708661568, 0.000000000000000000 ) ) ;
#1848 = AXIS2_PLACEMENT_3D ( 'NONE', #490, #13408, #411 ) ;
#1849 = CARTESIAN_POINT ( 'NONE',  ( 8.678599364036360127E-17, 0.000000000000000000, 0.7086614173228346081 ) ) ;
#1850 = CARTESIAN_POINT ( 'NONE',  ( -2.090430055232860962, -1.869646201002890251, -0.08681428844356724184 ) ) ;
#1851 = VECTOR ( 'NONE', #12251, 39.37007874015748143 ) ;
#1852 = ORIENTED_EDGE ( 'NONE', *, *, #11199, .T. ) ;
#1853 = ORIENTED_EDGE ( 'NONE', *, *, #9622, .F. ) ;
#1854 = ORIENTED_EDGE ( 'NONE', *, *, #11237, .T. ) ;
#1855 = ORIENTED_EDGE ( 'NONE', *, *, #12657, .T. ) ;
#1856 = EDGE_CURVE ( 'NONE', #3129, #1004, #1047, .T. ) ;
#1857 = AXIS2_PLACEMENT_3D ( 'NONE', #7340, #3912, #3990 ) ;
#1858 = EDGE_CURVE ( 'NONE', #6593, #2728, #4786, .T. ) ;
#1859 = CARTESIAN_POINT ( 'NONE',  ( -0.5412478373021294420, 1.346456692913385877, 0.2362233606508100381 ) ) ;
#1860 = AXIS2_PLACEMENT_3D ( 'NONE', #13071, #14329, #2497 ) ;
#1861 = DIRECTION ( 'NONE',  ( -0.8660254037844395958, 0.000000000000000000, 0.4999999999999982236 ) ) ;
#1862 = TOROIDAL_SURFACE ( 'NONE', #7355, 0.007874015748031495954, 0.003937007874015747977 ) ;
#1863 = CARTESIAN_POINT ( 'NONE',  ( 0.000000000000000000, 2.637795275590551825, 0.03937007874015747977 ) ) ;
#1864 = CIRCLE ( 'NONE', #12627, 0.003937007874015754916 ) ;
#1865 = CARTESIAN_POINT ( 'NONE',  ( 0.2681506793018588186, -0.4881889763779528324, 0.03207310886168001501 ) ) ;
#1866 = AXIS2_PLACEMENT_3D ( 'NONE', #8561, #10998, #7390 ) ;
#1867 = CARTESIAN_POINT ( 'NONE',  ( -1.352291563234457650, 0.1355266887446167634, 0.05905511811023622659 ) ) ;
#1868 = EDGE_CURVE ( 'NONE', #1163, #2262, #4696, .T. ) ;
#1869 = CARTESIAN_POINT ( 'NONE',  ( 0.09842519685044820443, -0.4881889763779528324, -0.5870514566507987197 ) ) ;
#1870 = CARTESIAN_POINT ( 'NONE',  ( -1.181102362204724310, 0.1279527559055117225, 0.02952755905511811330 ) ) ;
#1871 = DIRECTION ( 'NONE',  ( 0.000000000000000000, 0.000000000000000000, 1.000000000000000000 ) ) ;
#1872 = CARTESIAN_POINT ( 'NONE',  ( -1.934019134851861166, -2.845595952726013067, -0.1617770776497191865 ) ) ;
#1873 = VERTEX_POINT ( 'NONE', #4487 ) ;
#1874 = LINE ( 'NONE', #2099, #14951 ) ;
#1875 = CIRCLE ( 'NONE', #8892, 0.03937007874015761161 ) ;
#1876 = AXIS2_PLACEMENT_3D ( 'NONE', #1136, #5888, #13894 ) ;
#1877 = VECTOR ( 'NONE', #11584, 39.37007874015748143 ) ;
#1878 = ORIENTED_EDGE ( 'NONE', *, *, #5390, .T. ) ;
#1879 = VERTEX_POINT ( 'NONE', #1276 ) ;
#1880 = CIRCLE ( 'NONE', #3130, 0.007874015748031516770 ) ;
#1881 = UNCERTAINTY_MEASURE_WITH_UNIT (LENGTH_MEASURE( 1.000000000000000082E-05 ), #1593, 'distance_accuracy_value', 'NONE');
#1882 = ORIENTED_EDGE ( 'NONE', *, *, #4444, .T. ) ;
#1883 = CARTESIAN_POINT ( 'NONE',  ( -1.352291563234457650, 0.1355266887446167634, -0.03937007874015747977 ) ) ;
#1884 = CIRCLE ( 'NONE', #12650, 0.01968503937007879193 ) ;
#1885 = AXIS2_PLACEMENT_3D ( 'NONE', #4955, #3711, #7457 ) ;
#1886 = CIRCLE ( 'NONE', #3887, 0.05905511811023625435 ) ;
#1887 = DIRECTION ( 'NONE',  ( -0.000000000000000000, -1.000000000000000000, -0.000000000000000000 ) ) ;
#1888 = DIRECTION ( 'NONE',  ( 0.000000000000000000, 0.000000000000000000, -1.000000000000000000 ) ) ;
#1889 = EDGE_CURVE ( 'NONE', #13559, #1223, #13696, .T. ) ;
#1890 = DIRECTION ( 'NONE',  ( 0.000000000000000000, 0.000000000000000000, -1.000000000000000000 ) ) ;
#1891 = CARTESIAN_POINT ( 'NONE',  ( 0.2642136714278430776, -0.4921259842519685179, 0.03889220652927401906 ) ) ;
#1892 = TOROIDAL_SURFACE ( 'NONE', #9402, 0.04330708661417329020, 0.003937007874015747977 ) ;
#1893 = DIRECTION ( 'NONE',  ( 0.000000000000000000, 0.000000000000000000, -1.000000000000000000 ) ) ;
#1894 = ORIENTED_EDGE ( 'NONE', *, *, #10527, .F. ) ;
#1895 = CARTESIAN_POINT ( 'NONE',  ( -1.990519559797095939, -2.601568177549060668, 0.1382274484396485426 ) ) ;
#1896 = CARTESIAN_POINT ( 'NONE',  ( 0.5905511811023622659, -0.2952755905511811330, -0.3797276218561363992 ) ) ;
#1897 = ADVANCED_FACE ( 'NONE', ( #6913 ), #3399, .T. ) ;
#1898 = CYLINDRICAL_SURFACE ( 'NONE', #8851, 0.007874015748031516770 ) ;
#1899 = ORIENTED_EDGE ( 'NONE', *, *, #12865, .T. ) ;
#1900 = ADVANCED_FACE ( 'NONE', ( #14671 ), #3775, .F. ) ;
#1901 = DIRECTION ( 'NONE',  ( 0.4999999999999995004, 0.000000000000000000, 0.8660254037844390407 ) ) ;
#1902 = TOROIDAL_SURFACE ( 'NONE', #2145, 0.5590551181102362266, 0.007874015748031495954 ) ;
#1903 = CONICAL_SURFACE ( 'NONE', #11919, 0.05298991407461853265, 1.279339532317029349 ) ;
#1904 = AXIS2_PLACEMENT_3D ( 'NONE', #11701, #15223, #3394 ) ;
#1905 = VERTEX_POINT ( 'NONE', #3929 ) ;
#1906 = ORIENTED_EDGE ( 'NONE', *, *, #13596, .F. ) ;
#1907 = AXIS2_PLACEMENT_3D ( 'NONE', #12265, #5984, #6048 ) ;
#1908 = PRODUCT ( 'Spider', 'Spider', '', ( #9038 ) ) ;
#1909 = LINE ( 'NONE', #11533, #4663 ) ;
#1910 = DIRECTION ( 'NONE',  ( 1.000000000000000000, 0.000000000000000000, 0.000000000000000000 ) ) ;
#1911 = CARTESIAN_POINT ( 'NONE',  ( -0.02897706919690611060, 0.1719584017861309766, -0.007005952774887016718 ) ) ;
#1912 = DIRECTION ( 'NONE',  ( -0.5000000000000004441, -0.000000000000000000, -0.8660254037844384856 ) ) ;
#1913 = DIRECTION ( 'NONE',  ( -1.000000000000000222, -8.326672684688674053E-17, 1.665334536937734811E-15 ) ) ;
#1914 = DIRECTION ( 'NONE',  ( 0.5000000000000035527, 0.000000000000000000, -0.8660254037844365982 ) ) ;
#1915 = AXIS2_PLACEMENT_3D ( 'NONE', #11004, #7251, #443 ) ;
#1916 = CARTESIAN_POINT ( 'NONE',  ( -1.572611271870161920, 0.1123963381035097825, 0.05997718891489349502 ) ) ;
#1917 = ORIENTED_EDGE ( 'NONE', *, *, #10166, .F. ) ;
#1918 = DIRECTION ( 'NONE',  ( -0.5984233124757303290, -0.8011800915434521553, 0.000000000000000000 ) ) ;
#1919 = CARTESIAN_POINT ( 'NONE',  ( -0.06692913385815757454, -0.4921259842519685179, -2.418823744386252084E-17 ) ) ;
#1920 = VECTOR ( 'NONE', #8565, 39.37007874015748143 ) ;
#1921 = LINE ( 'NONE', #12568, #14937 ) ;
#1922 = VERTEX_POINT ( 'NONE', #8711 ) ;
#1923 = ORIENTED_EDGE ( 'NONE', *, *, #950, .T. ) ;
#1924 = ORIENTED_EDGE ( 'NONE', *, *, #13619, .F. ) ;
#1925 = VECTOR ( 'NONE', #7524, 39.37007874015748854 ) ;
#1926 = CARTESIAN_POINT ( 'NONE',  ( -0.2681506793016945611, -0.1023622047244094474, 0.03207310886158502850 ) ) ;
#1927 = CARTESIAN_POINT ( 'NONE',  ( -1.981861006536024927, -2.839447705569534186, 0.1644972641858484519 ) ) ;
#1928 = CARTESIAN_POINT ( 'NONE',  ( 0.1181102362204724116, 2.448818897637795367, 0.03937007874015747977 ) ) ;
#1929 = CARTESIAN_POINT ( 'NONE',  ( -1.962410390378336977, -2.889890278503658649, -0.1129139997297211734 ) ) ;
#1930 = FACE_OUTER_BOUND ( 'NONE', #9258, .T. ) ;
#1931 = AXIS2_PLACEMENT_3D ( 'NONE', #3119, #14876, #8931 ) ;
#1932 = FACE_OUTER_BOUND ( 'NONE', #10268, .T. ) ;
#1933 = EDGE_CURVE ( 'NONE', #2868, #2979, #13948, .T. ) ;
#1934 = CARTESIAN_POINT ( 'NONE',  ( 0.4854723491485768982, 1.043263280880422528, 0.3484785681409844904 ) ) ;
#1935 = CARTESIAN_POINT ( 'NONE',  ( -2.087366308036623597, -1.727041808514125254, -0.08405390020912445470 ) ) ;
#1936 = AXIS2_PLACEMENT_3D ( 'NONE', #13291, #4916, #13062 ) ;
#1937 = EDGE_CURVE ( 'NONE', #7178, #3700, #13839, .T. ) ;
#1938 = ORIENTED_EDGE ( 'NONE', *, *, #1367, .F. ) ;
#1939 = EDGE_LOOP ( 'NONE', ( #11995, #12572, #13977, #12235 ) ) ;
#1940 = AXIS2_PLACEMENT_3D ( 'NONE', #2450, #5723, #4726 ) ;
#1941 = ORIENTED_EDGE ( 'NONE', *, *, #13477, .T. ) ;
#1942 = VERTEX_POINT ( 'NONE', #13486 ) ;
#1943 = EDGE_CURVE ( 'NONE', #4794, #8918, #951, .T. ) ;
#1944 = VECTOR ( 'NONE', #10157, 39.37007874015748143 ) ;
#1945 = CARTESIAN_POINT ( 'NONE',  ( -0.06299212598414166697, -0.2952755905511811330, -0.4190977005962941426 ) ) ;
#1946 = CYLINDRICAL_SURFACE ( 'NONE', #2115, 0.1476377952755905942 ) ;
#1947 = AXIS2_PLACEMENT_3D ( 'NONE', #11990, #9709, #14317 ) ;
#1948 = DIRECTION ( 'NONE',  ( 0.000000000000000000, 0.000000000000000000, 1.000000000000000000 ) ) ;
#1949 = DIRECTION ( 'NONE',  ( -1.224646799147343593E-16, 0.000000000000000000, -1.000000000000000000 ) ) ;
#1950 = CARTESIAN_POINT ( 'NONE',  ( -0.06154672136187318982, -0.1666784585780658190, -0.05764611276129244510 ) ) ;
#1951 = CARTESIAN_POINT ( 'NONE',  ( 0.000000000000000000, 0.007874015748031480341, 0.000000000000000000 ) ) ;
#1952 = FACE_OUTER_BOUND ( 'NONE', #942, .T. ) ;
#1953 = ORIENTED_EDGE ( 'NONE', *, *, #5096, .T. ) ;
#1954 = DIRECTION ( 'NONE',  ( -0.5000000000000035527, -0.000000000000000000, 0.8660254037844365982 ) ) ;
#1955 = ADVANCED_FACE ( 'NONE', ( #6188 ), #10980, .F. ) ;
#1956 = B_SPLINE_CURVE_WITH_KNOTS ( 'NONE', 3,
 ( #10535, #15314, #9000, #7074 ),
 .UNSPECIFIED., .F., .F.,
 ( 4, 4 ),
 ( 0.000000000000000000, 0.005704847486038692669 ),
 .UNSPECIFIED. ) ;
#1957 = CARTESIAN_POINT ( 'NONE',  ( 0.000000000000000000, 0.5984251968503937480, 0.000000000000000000 ) ) ;
#1958 = AXIS2_PLACEMENT_3D ( 'NONE', #13009, #15443, #84 ) ;
#1959 = EDGE_CURVE ( 'NONE', #12255, #14974, #6560, .T. ) ;
#1960 = ORIENTED_EDGE ( 'NONE', *, *, #6942, .T. ) ;
#1961 = EDGE_LOOP ( 'NONE', ( #12312, #10307, #10096, #7268 ) ) ;
#1962 = AXIS2_PLACEMENT_3D ( 'NONE', #12007, #1263, #7351 ) ;
#1963 = ADVANCED_FACE ( 'NONE', ( #13867 ), #10265, .F. ) ;
#1964 = EDGE_CURVE ( 'NONE', #6858, #12158, #10700, .T. ) ;
#1965 = ORIENTED_EDGE ( 'NONE', *, *, #116, .T. ) ;
#1966 = CYLINDRICAL_SURFACE ( 'NONE', #13124, 0.003937007874015724558 ) ;
#1967 = CIRCLE ( 'NONE', #6417, 0.003937007874015724558 ) ;
#1968 = DIRECTION ( 'NONE',  ( 0.000000000000000000, 0.000000000000000000, -1.000000000000000000 ) ) ;
#1969 = CARTESIAN_POINT ( 'NONE',  ( 0.000000000000000000, 1.338582677165354395, -0.5984251968503937480 ) ) ;
#1970 = DIRECTION ( 'NONE',  ( 0.8144815189573204606, -0.5801894994542525774, 0.000000000000000000 ) ) ;
#1971 = DIRECTION ( 'NONE',  ( -1.060575238724907285E-16, 1.000000000000000000, 6.123233995736761105E-17 ) ) ;
#1972 = LINE ( 'NONE', #8155, #5624 ) ;
#1973 = ORIENTED_EDGE ( 'NONE', *, *, #14321, .T. ) ;
#1974 = CARTESIAN_POINT ( 'NONE',  ( -0.5615510810874360104, -0.09448818897637796532, 0.2014679098129269208 ) ) ;
#1975 = DIRECTION ( 'NONE',  ( 1.000000000000000000, -0.000000000000000000, 1.224646799147353207E-16 ) ) ;
#1976 = CARTESIAN_POINT ( 'NONE',  ( -0.4787089944775287931, 1.040121464703355647, 0.3474236500605662470 ) ) ;
#1977 = CARTESIAN_POINT ( 'NONE',  ( -1.185590514512987692, 0.3351394516327975692, 0.05695402452142334787 ) ) ;
#1978 = ORIENTED_EDGE ( 'NONE', *, *, #7205, .F. ) ;
#1979 = DIRECTION ( 'NONE',  ( -1.000000000000000000, -1.734723475976807094E-14, 0.000000000000000000 ) ) ;
#1980 = ORIENTED_EDGE ( 'NONE', *, *, #12028, .F. ) ;
#1981 = EDGE_CURVE ( 'NONE', #10078, #1174, #7695, .T. ) ;
#1982 = ADVANCED_FACE ( 'NONE', ( #3140 ), #941, .T. ) ;
#1983 = ORIENTED_EDGE ( 'NONE', *, *, #7087, .T. ) ;
#1984 = DIRECTION ( 'NONE',  ( 1.000000000000000000, 1.734723475976802677E-14, 0.000000000000000000 ) ) ;
#1985 = DIRECTION ( 'NONE',  ( 0.8660254037844362651, 0.000000000000000000, -0.5000000000000041078 ) ) ;
#1986 = EDGE_CURVE ( 'NONE', #13529, #10725, #1443, .T. ) ;
#1987 = CARTESIAN_POINT ( 'NONE',  ( -0.02344272421051980110, 0.1505984473677600133, -0.03705048130896489156 ) ) ;
#1988 = CARTESIAN_POINT ( 'NONE',  ( -1.181102362204724310, -0.1279527559055117225, -0.02559055118110236185 ) ) ;
#1989 = CYLINDRICAL_SURFACE ( 'NONE', #6663, 0.003937007874015721089 ) ;
#1990 = CARTESIAN_POINT ( 'NONE',  ( -0.1968503937007873295, -0.02638708502139245141, 0.05905511811023622659 ) ) ;
#1991 = ORIENTED_EDGE ( 'NONE', *, *, #14391, .T. ) ;
#1992 = DIRECTION ( 'NONE',  ( 0.000000000000000000, 0.000000000000000000, 1.000000000000000000 ) ) ;
#1993 = CARTESIAN_POINT ( 'NONE',  ( -0.06692913385815728311, -0.2952755905511811330, -0.4190977005962941426 ) ) ;
#1994 = DIRECTION ( 'NONE',  ( 0.000000000000000000, 0.000000000000000000, 1.000000000000000000 ) ) ;
#1995 = ORIENTED_EDGE ( 'NONE', *, *, #12608, .F. ) ;
#1996 = DIRECTION ( 'NONE',  ( 1.000000000000000000, 0.000000000000000000, 0.000000000000000000 ) ) ;
#1997 = ORIENTED_EDGE ( 'NONE', *, *, #505, .F. ) ;
#1998 = ORIENTED_EDGE ( 'NONE', *, *, #7410, .F. ) ;
#1999 = EDGE_CURVE ( 'NONE', #2901, #3536, #12946, .T. ) ;
#2000 = CARTESIAN_POINT ( 'NONE',  ( 0.000000000000000000, 0.4133858267716535306, 0.000000000000000000 ) ) ;
#2001 = CYLINDRICAL_SURFACE ( 'NONE', #14089, 0.003937007874015724558 ) ;
#2002 = DIRECTION ( 'NONE',  ( 4.336808689942025625E-15, 0.000000000000000000, 1.000000000000000000 ) ) ;
#2003 = FACE_OUTER_BOUND ( 'NONE', #7442, .T. ) ;
#2004 = LINE ( 'NONE', #823, #344 ) ;
#2005 = CARTESIAN_POINT ( 'NONE',  ( -1.945459748359984697, -2.745801194614593488, -0.1561691687464119294 ) ) ;
#2006 = ORIENTED_EDGE ( 'NONE', *, *, #6413, .F. ) ;
#2007 = ORIENTED_EDGE ( 'NONE', *, *, #5272, .T. ) ;
#2008 = EDGE_LOOP ( 'NONE', ( #12285, #8123, #9758, #5973, #12336, #12520 ) ) ;
#2009 = ORIENTED_EDGE ( 'NONE', *, *, #10583, .T. ) ;
#2010 = DIRECTION ( 'NONE',  ( 0.000000000000000000, 0.000000000000000000, -1.000000000000000000 ) ) ;
#2011 = LINE ( 'NONE', #9233, #13122 ) ;
#2012 = EDGE_CURVE ( 'NONE', #8683, #13359, #3194, .T. ) ;
#2013 = DIRECTION ( 'NONE',  ( -0.000000000000000000, 1.000000000000000000, -0.000000000000000000 ) ) ;
#2014 = CARTESIAN_POINT ( 'NONE',  ( 0.000000000000000000, 0.06496062992125986590, 0.000000000000000000 ) ) ;
#2015 = DIRECTION ( 'NONE',  ( 0.8660254037844383745, 0.000000000000000000, 0.5000000000000004441 ) ) ;
#2016 = CARTESIAN_POINT ( 'NONE',  ( -1.182291936362779738, 0.3416838286731589402, 0.04963174987406704375 ) ) ;
#2017 = CARTESIAN_POINT ( 'NONE',  ( -1.932501772242613214, -2.783625412848802938, -0.1565638296097948412 ) ) ;
#2018 = ORIENTED_EDGE ( 'NONE', *, *, #5129, .F. ) ;
#2019 = LINE ( 'NONE', #5531, #11444 ) ;
#2020 = EDGE_CURVE ( 'NONE', #13529, #10010, #11280, .T. ) ;
#2021 = DIRECTION ( 'NONE',  ( 0.000000000000000000, 0.000000000000000000, -1.000000000000000000 ) ) ;
#2022 = PRODUCT_DEFINITION_SHAPE ( 'NONE', 'NONE',  #15484 ) ;
#2023 = ORIENTED_EDGE ( 'NONE', *, *, #13199, .F. ) ;
#2024 = ORIENTED_EDGE ( 'NONE', *, *, #9588, .T. ) ;
#2025 = ORIENTED_EDGE ( 'NONE', *, *, #5981, .T. ) ;
#2026 = DIRECTION ( 'NONE',  ( -1.000000000000000000, 0.000000000000000000, 0.000000000000000000 ) ) ;
#2027 = EDGE_CURVE ( 'NONE', #4567, #7635, #6431, .T. ) ;
#2028 = EDGE_CURVE ( 'NONE', #14862, #11768, #10451, .T. ) ;
#2029 = FACE_OUTER_BOUND ( 'NONE', #14239, .T. ) ;
#2030 = CARTESIAN_POINT ( 'NONE',  ( -1.933898541317984776, -2.925115481561290309, 0.09044664578863767512 ) ) ;
#2031 = FACE_BOUND ( 'NONE', #5280, .T. ) ;
#2032 = CARTESIAN_POINT ( 'NONE',  ( -0.4861941749621833675, 1.043307086614173373, 0.3488953144687877983 ) ) ;
#2033 = EDGE_LOOP ( 'NONE', ( #4734, #13202, #8370, #9239, #1161 ) ) ;
#2034 = CARTESIAN_POINT ( 'NONE',  ( 0.000000000000000000, -0.4921259842519685179, 0.2083147301385909200 ) ) ;
#2035 = EDGE_CURVE ( 'NONE', #2747, #2525, #10658, .T. ) ;
#2036 = DIRECTION ( 'NONE',  ( -4.292327424963333000E-16, -1.000000000000000000, -2.478176394252540219E-16 ) ) ;
#2037 = CARTESIAN_POINT ( 'NONE',  ( -0.002500327830562678200, 0.1532658568795227105, 0.000000000000000000 ) ) ;
#2038 = CARTESIAN_POINT ( 'NONE',  ( -1.580259682937477539, 0.1018956540319142512, 0.04477369844320258641 ) ) ;
#2039 = ORIENTED_EDGE ( 'NONE', *, *, #4192, .F. ) ;
#2040 = FACE_OUTER_BOUND ( 'NONE', #8942, .T. ) ;
#2041 = ORIENTED_EDGE ( 'NONE', *, *, #2654, .F. ) ;
#2042 = ORIENTED_EDGE ( 'NONE', *, *, #11662, .F. ) ;
#2043 = ORIENTED_EDGE ( 'NONE', *, *, #5220, .F. ) ;
#2044 = EDGE_CURVE ( 'NONE', #12219, #14791, #12931, .T. ) ;
#2045 = DIRECTION ( 'NONE',  ( 0.000000000000000000, 0.000000000000000000, -1.000000000000000000 ) ) ;
#2046 = CARTESIAN_POINT ( 'NONE',  ( -0.5379290338433415641, -0.09842519685039370636, 0.2423824958184910838 ) ) ;
#2047 = EDGE_CURVE ( 'NONE', #924, #8242, #12203, .T. ) ;
#2048 = DIRECTION ( 'NONE',  ( 0.000000000000000000, 1.000000000000000000, 0.000000000000000000 ) ) ;
#2049 = ITEM_DEFINED_TRANSFORMATION ( 'NONE', 'NONE', #6600,  #11481 ) ;
#2050 = PLANE ( 'NONE',  #4686 ) ;
#2051 = CARTESIAN_POINT ( 'NONE',  ( 0.4141303577462121521, -0.2952755905511811330, 0.1209005806194717869 ) ) ;
#2052 = ORIENTED_EDGE ( 'NONE', *, *, #3042, .F. ) ;
#2053 = CARTESIAN_POINT ( 'NONE',  ( -1.276200637803905691, -0.1988000726501942539, -0.08366141732283455257 ) ) ;
#2054 = ADVANCED_FACE ( 'NONE', ( #8298 ), #10569, .F. ) ;
#2055 = CARTESIAN_POINT ( 'NONE',  ( 0.000000000000000000, 0.003937007874015749712, 0.000000000000000000 ) ) ;
#2056 = DIRECTION ( 'NONE',  ( 1.000000000000000000, 0.000000000000000000, 0.000000000000000000 ) ) ;
#2057 = DIRECTION ( 'NONE',  ( 0.000000000000000000, -1.000000000000000000, -0.000000000000000000 ) ) ;
#2058 = CARTESIAN_POINT ( 'NONE',  ( -1.181102362204724310, -0.1240157480314959815, 0.02952755905511811330 ) ) ;
#2059 = EDGE_LOOP ( 'NONE', ( #10098, #11722, #12011, #10474 ) ) ;
#2060 = ORIENTED_EDGE ( 'NONE', *, *, #3193, .F. ) ;
#2061 = ADVANCED_FACE ( 'NONE', ( #13008 ), #7043, .F. ) ;
#2062 = CARTESIAN_POINT ( 'NONE',  ( 0.5860051159906326523, -0.09842519685039370636, 0.1591122789105293700 ) ) ;
#2063 = EDGE_LOOP ( 'NONE', ( #13034, #5955, #2082, #8899 ) ) ;
#2064 = ORIENTED_EDGE ( 'NONE', *, *, #8846, .F. ) ;
#2065 = ORIENTED_EDGE ( 'NONE', *, *, #10422, .T. ) ;
#2066 = AXIS2_PLACEMENT_3D ( 'NONE', #3098, #14852, #2862 ) ;
#2067 = CARTESIAN_POINT ( 'NONE',  ( -0.06299212598414173636, -0.1023622047244094474, -0.2366577558633980449 ) ) ;
#2068 = LINE ( 'NONE', #6842, #11331 ) ;
#2069 =( NAMED_UNIT ( * ) PLANE_ANGLE_UNIT ( ) SI_UNIT ( $, .RADIAN. ) );
#2070 = CARTESIAN_POINT ( 'NONE',  ( -1.137795275590550936, 0.000000000000000000, -0.02559055118110236185 ) ) ;
#2071 = CYLINDRICAL_SURFACE ( 'NONE', #10401, 0.1181102362204724532 ) ;
#2072 = EDGE_CURVE ( 'NONE', #3129, #2378, #9497, .T. ) ;
#2073 = DIRECTION ( 'NONE',  ( -0.8660254037844390407, 0.000000000000000000, 0.4999999999999994449 ) ) ;
#2074 = SPHERICAL_SURFACE ( 'NONE', #14586, 0.003937007874015747977 ) ;
#2075 = CARTESIAN_POINT ( 'NONE',  ( -0.06692913385815735250, -0.4881889763779528324, -0.5870514566507987197 ) ) ;
#2076 = CIRCLE ( 'NONE', #4078, 0.1574803149606299191 ) ;
#2077 = AXIS2_PLACEMENT_3D ( 'NONE', #4522, #9304, #2184 ) ;
#2078 = EDGE_CURVE ( 'NONE', #2233, #7918, #6989, .T. ) ;
#2079 = VERTEX_POINT ( 'NONE', #954 ) ;
#2080 = CIRCLE ( 'NONE', #10829, 0.003937007874015741038 ) ;
#2081 = ADVANCED_FACE ( 'NONE', ( #8058 ), #5683, .T. ) ;
#2082 = ORIENTED_EDGE ( 'NONE', *, *, #49, .F. ) ;
#2083 = AXIS2_PLACEMENT_3D ( 'NONE', #15033, #1723, #481 ) ;
#2084 = ORIENTED_EDGE ( 'NONE', *, *, #11237, .F. ) ;
#2085 = ORIENTED_EDGE ( 'NONE', *, *, #260, .T. ) ;
#2086 = DIRECTION ( 'NONE',  ( 1.000000000000000000, -0.000000000000000000, 1.224646799147353207E-16 ) ) ;
#2087 = CARTESIAN_POINT ( 'NONE',  ( -1.115439883890946726, -0.06270839865334708330, 0.1968503937007874127 ) ) ;
#2088 = AXIS2_PLACEMENT_3D ( 'NONE', #6059, #4909, #3739 ) ;
#2089 = DIRECTION ( 'NONE',  ( -1.000000000000000000, 0.000000000000000000, 0.000000000000000000 ) ) ;
#2090 = AXIS2_PLACEMENT_3D ( 'NONE', #4200, #12434, #13517 ) ;
#2091 = CARTESIAN_POINT ( 'NONE',  ( -0.02897706919691097130, 0.1719584017861302827, 0.007005952774883386809 ) ) ;
#2092 = AXIS2_PLACEMENT_3D ( 'NONE', #14384, #11220, #7175 ) ;
#2093 = CARTESIAN_POINT ( 'NONE',  ( -1.527714331928839098, 0.2380340132385416752, 0.03937007874015747977 ) ) ;
#2094 = CARTESIAN_POINT ( 'NONE',  ( -0.002500327830563101039, -0.1605493263772690415, 0.000000000000000000 ) ) ;
#2095 = AXIS2_PLACEMENT_3D ( 'NONE', #3483, #14355, #7295 ) ;
#2096 = DIRECTION ( 'NONE',  ( -0.000000000000000000, 0.000000000000000000, 1.000000000000000000 ) ) ;
#2097 = CARTESIAN_POINT ( 'NONE',  ( -1.898397756988851715, -2.875673457072045025, -0.1127397473705673697 ) ) ;
#2098 = VERTEX_POINT ( 'NONE', #4537 ) ;
#2099 = CARTESIAN_POINT ( 'NONE',  ( 0.1574803149606299191, -0.09448818897637796532, -0.5909884645248143498 ) ) ;
#2100 = CARTESIAN_POINT ( 'NONE',  ( 1.309055118110236116, 4.044111181948214319E-16, 0.02559055118110236185 ) ) ;
#2101 = EDGE_LOOP ( 'NONE', ( #8506, #13736, #6923, #11840 ) ) ;
#2102 = EDGE_LOOP ( 'NONE', ( #4188, #14365, #1075, #8468 ) ) ;
#2103 = AXIS2_PLACEMENT_3D ( 'NONE', #1371, #11967, #9766 ) ;
#2104 = CIRCLE ( 'NONE', #11611, 0.6614173228346456046 ) ;
#2105 = CIRCLE ( 'NONE', #117, 0.003937007874015758385 ) ;
#2106 = TOROIDAL_SURFACE ( 'NONE', #1114, 0.04330708661417328326, 0.003937007874015747977 ) ;
#2107 = VERTEX_POINT ( 'NONE', #5062 ) ;
#2108 = AXIS2_PLACEMENT_3D ( 'NONE', #1127, #11850, #10749 ) ;
#2109 = DIRECTION ( 'NONE',  ( 0.000000000000000000, 1.000000000000000000, 0.000000000000000000 ) ) ;
#2110 = EDGE_LOOP ( 'NONE', ( #4960, #15372, #7655, #222 ) ) ;
#2111 = DIRECTION ( 'NONE',  ( 0.000000000000000000, 0.000000000000000000, -1.000000000000000000 ) ) ;
#2112 = CARTESIAN_POINT ( 'NONE',  ( -1.933937248003420262, -2.925008321567649894, -0.09063602501266794509 ) ) ;
#2113 = AXIS2_PLACEMENT_3D ( 'NONE', #15147, #12871, #10596 ) ;
#2114 = DIRECTION ( 'NONE',  ( -0.000000000000000000, -0.000000000000000000, -1.000000000000000000 ) ) ;
#2115 = AXIS2_PLACEMENT_3D ( 'NONE', #11498, #9153, #931 ) ;
#2116 = TOROIDAL_SURFACE ( 'NONE', #9875, 0.5590551181102362266, 0.007874015748031495954 ) ;
#2117 = VERTEX_POINT ( 'NONE', #14562 ) ;
#2118 = CARTESIAN_POINT ( 'NONE',  ( -0.1968503937007873295, -0.02638708502139245141, -0.03937007874015747977 ) ) ;
#2119 = CYLINDRICAL_SURFACE ( 'NONE', #12126, 0.003937007874015724558 ) ;
#2120 = AXIS2_PLACEMENT_3D ( 'NONE', #13185, #3705, #9809 ) ;
#2121 = CARTESIAN_POINT ( 'NONE',  ( -0.004690417658706403335, 0.1529805375610461537, 0.008482181431098844218 ) ) ;
#2122 = DIRECTION ( 'NONE',  ( 1.000000000000000000, 0.000000000000000000, 0.000000000000000000 ) ) ;
#2123 = ORIENTED_EDGE ( 'NONE', *, *, #10480, .T. ) ;
#2124 = ADVANCED_FACE ( 'NONE', ( #3823 ), #14119, .T. ) ;
#2125 = CARTESIAN_POINT ( 'NONE',  ( -0.1259842519685039353, 2.448818897637795367, 0.000000000000000000 ) ) ;
#2126 = EDGE_CURVE ( 'NONE', #10256, #4318, #9792, .T. ) ;
#2127 = ORIENTED_EDGE ( 'NONE', *, *, #3979, .F. ) ;
#2129 = ORIENTED_EDGE ( 'NONE', *, *, #12254, .F. ) ;
#2128 = CIRCLE ( 'NONE', #11391, 0.01968503937007871907 ) ;
#2130 = CIRCLE ( 'NONE', #5619, 0.007874015748031449116 ) ;
#2131 = ORIENTED_EDGE ( 'NONE', *, *, #9016, .F. ) ;
#2132 = AXIS2_PLACEMENT_3D ( 'NONE', #12060, #10877, #14557 ) ;
#2133 = ADVANCED_FACE ( 'NONE', ( #8463 ), #14902, .T. ) ;
#2134 = DIRECTION ( 'NONE',  ( 0.000000000000000000, -1.000000000000000000, 2.183568011719057743E-16 ) ) ;
#2135 = CARTESIAN_POINT ( 'NONE',  ( -0.3294846884549019750, -0.2952755905511811330, 0.2675111804726950648 ) ) ;
#2136 = VECTOR ( 'NONE', #12914, 39.37007874015748143 ) ;
#2137 = PLANE ( 'NONE',  #13354 ) ;
#2138 = DIRECTION ( 'NONE',  ( 1.000000000000000000, -0.000000000000000000, -0.000000000000000000 ) ) ;
#2139 = CONTEXT_DEPENDENT_SHAPE_REPRESENTATION ( #14510, #7429 ) ;
#2140 = DIRECTION ( 'NONE',  ( 0.000000000000000000, 0.000000000000000000, -1.000000000000000000 ) ) ;
#2141 = LINE ( 'NONE', #11539, #14134 ) ;
#2142 = ORIENTED_EDGE ( 'NONE', *, *, #12322, .T. ) ;
#2143 = CARTESIAN_POINT ( 'NONE',  ( -0.05905511811023622659, 1.190944881889763884, -0.8267716535433072833 ) ) ;
#2144 = CARTESIAN_POINT ( 'NONE',  ( -1.576201932089460689, 0.1075912864651075579, 0.06349180857236520759 ) ) ;
#2145 = AXIS2_PLACEMENT_3D ( 'NONE', #4825, #5837, #12995 ) ;
#2146 = AXIS2_PLACEMENT_3D ( 'NONE', #774, #418, #9164 ) ;
#2147 = DIRECTION ( 'NONE',  ( 0.000000000000000000, 1.000000000000000000, 2.212657494868377674E-16 ) ) ;
#2148 = AXIS2_PLACEMENT_3D ( 'NONE', #2561, #14558, #8604 ) ;
#2149 = ADVANCED_FACE ( 'NONE', ( #6084, #12231 ), #173, .T. ) ;
#2150 = VERTEX_POINT ( 'NONE', #3686 ) ;
#2151 = CIRCLE ( 'NONE', #10901, 0.003937007874015724558 ) ;
#2152 = EDGE_CURVE ( 'NONE', #13232, #6564, #1580, .T. ) ;
#2153 = ORIENTED_EDGE ( 'NONE', *, *, #7341, .T. ) ;
#2154 = CARTESIAN_POINT ( 'NONE',  ( 0.6864776960422569463, 1.190944881889763884, 0.4645290592786023298 ) ) ;
#2155 = ORIENTED_EDGE ( 'NONE', *, *, #2493, .T. ) ;
#2156 = EDGE_LOOP ( 'NONE', ( #8278, #14220, #11687 ) ) ;
#2157 = EDGE_CURVE ( 'NONE', #5195, #14360, #6573, .T. ) ;
#2158 = EDGE_LOOP ( 'NONE', ( #11810, #6074, #5323, #11592 ) ) ;
#2159 = AXIS2_PLACEMENT_3D ( 'NONE', #10514, #4404, #6745 ) ;
#2160 = DIRECTION ( 'NONE',  ( 0.5000000000000008882, 0.000000000000000000, -0.8660254037844381525 ) ) ;
#2161 = VECTOR ( 'NONE', #11412, 39.37007874015748143 ) ;
#2162 = AXIS2_PLACEMENT_3D ( 'NONE', #2880, #5148, #389 ) ;
#2163 = DIRECTION ( 'NONE',  ( -8.673617379884029309E-17, 1.000000000000000000, 0.000000000000000000 ) ) ;
#2164 = CARTESIAN_POINT ( 'NONE',  ( -1.957251767099916107, -2.772329397582958599, 0.1771653543307079026 ) ) ;
#2165 = CARTESIAN_POINT ( 'NONE',  ( -0.1724006475077544398, -0.4881889763779528324, 0.1768186671464649917 ) ) ;
#2166 = AXIS2_PLACEMENT_3D ( 'NONE', #5800, #15230, #2224 ) ;
#2167 = CARTESIAN_POINT ( 'NONE',  ( -0.06692913385815749128, -0.09842519685039370636, -0.2377126739438355507 ) ) ;
#2168 = CARTESIAN_POINT ( 'NONE',  ( -0.1062992125983150127, -0.4881889763779528324, -0.2482618547482104143 ) ) ;
#2169 = LINE ( 'NONE', #1870, #11843 ) ;
#2170 = CARTESIAN_POINT ( 'NONE',  ( -0.5576140732134202693, -0.4881889763779528324, 0.2082870074805209248 ) ) ;
#2171 = AXIS2_PLACEMENT_3D ( 'NONE', #10144, #9993, #14933 ) ;
#2172 = VERTEX_POINT ( 'NONE', #7507 ) ;
#2173 = ORIENTED_EDGE ( 'NONE', *, *, #7896, .F. ) ;
#2174 = ORIENTED_EDGE ( 'NONE', *, *, #11214, .F. ) ;
#2175 = VECTOR ( 'NONE', #10335, 39.37007874015748143 ) ;
#2176 = EDGE_LOOP ( 'NONE', ( #9345, #13334 ) ) ;
#2177 = EDGE_CURVE ( 'NONE', #9678, #8145, #5568, .T. ) ;
#2178 =( BOUNDED_SURFACE ( )  B_SPLINE_SURFACE ( 3, 2, ( 
 ( #3440, #3344, #14168 ),
 ( #15331, #6867, #14007 ),
 ( #11749, #14074, #12913 ),
 ( #5610, #6956, #4757 ),
 ( #1011, #3573, #15186 ),
 ( #1169, #8218, #5758 ),
 ( #10552, #139, #4594 ),
 ( #7098, #9234, #2091 ),
 ( #3268, #838, #10482 ),
 ( #9389, #2252, #14245 ) ),
 .UNSPECIFIED., .F., .F., .T. ) 
 B_SPLINE_SURFACE_WITH_KNOTS ( ( 4, 2, 2, 2, 4 ),
 ( 3, 3 ),
 ( 0.004868238565068924370, 0.005367227319713952817, 0.005866216074358981264, 0.006365204829004009711, 0.006864193583649038158 ),
 ( 0.000000000000000000, 1.000000000000000000 ),
 .UNSPECIFIED. ) 
 GEOMETRIC_REPRESENTATION_ITEM ( )  RATIONAL_B_SPLINE_SURFACE ( (
 ( 1.000000000000000000, 0.7071067811865474617, 1.000000000000000000),
 ( 1.000000000000000000, 0.7015640395779101368, 1.000000000000000000),
 ( 1.000000000000000000, 0.6956970733052191269, 1.000000000000000000),
 ( 1.000000000000000000, 0.6834122233792455647, 1.000000000000000000),
 ( 1.000000000000000000, 0.6772899333991025950, 1.000000000000000000),
 ( 1.000000000000000000, 0.6655724472122640512, 1.000000000000000000),
 ( 1.000000000000000000, 0.6602173990144353244, 1.000000000000000000),
 ( 1.000000000000000000, 0.6512508157287528743, 1.000000000000000000),
 ( 1.000000000000000000, 0.6477776718208990703, 1.000000000000000000),
 ( 1.000000000000000000, 0.6456929433798522799, 1.000000000000000000) ) ) 
 REPRESENTATION_ITEM ( '' )  SURFACE ( )  );
#2179 = CARTESIAN_POINT ( 'NONE',  ( 0.000000000000000000, 1.409448818897637956, 0.000000000000000000 ) ) ;
#2180 = LINE ( 'NONE', #5686, #4114 ) ;
#2181 =( GEOMETRIC_REPRESENTATION_CONTEXT ( 3 ) GLOBAL_UNCERTAINTY_ASSIGNED_CONTEXT ( ( #4064 ) ) GLOBAL_UNIT_ASSIGNED_CONTEXT ( ( #421, #4240, #14911 ) ) REPRESENTATION_CONTEXT ( 'NONE', 'WORKASPACE' ) );
#2182 = EDGE_CURVE ( 'NONE', #13463, #14839, #9592, .T. ) ;
#2183 = DIRECTION ( 'NONE',  ( -1.000000000000000000, 0.000000000000000000, 0.000000000000000000 ) ) ;
#2184 = DIRECTION ( 'NONE',  ( 1.000000000000000000, 0.000000000000000000, 0.000000000000000000 ) ) ;
#2185 = AXIS2_PLACEMENT_3D ( 'NONE', #7574, #12372, #3048 ) ;
#2186 = LINE ( 'NONE', #5761, #10407 ) ;
#2187 = VERTEX_POINT ( 'NONE', #3992 ) ;
#2188 = CARTESIAN_POINT ( 'NONE',  ( 0.06692913385832212347, -0.09842519685039370636, -0.5870514566507987197 ) ) ;
#2189 = FACE_OUTER_BOUND ( 'NONE', #2298, .T. ) ;
#2190 = DIRECTION ( 'NONE',  ( -1.000000000000000000, 0.000000000000000000, 0.000000000000000000 ) ) ;
#2191 = AXIS2_PLACEMENT_3D ( 'NONE', #3287, #8379, #9249 ) ;
#2192 = ORIENTED_EDGE ( 'NONE', *, *, #795, .T. ) ;
#2193 = ORIENTED_EDGE ( 'NONE', *, *, #5100, .T. ) ;
#2194 = CIRCLE ( 'NONE', #8440, 0.5905511811023621549 ) ;
#2195 = VERTEX_POINT ( 'NONE', #8766 ) ;
#2196 = AXIS2_PLACEMENT_3D ( 'NONE', #13193, #334, #11049 ) ;
#2197 = LINE ( 'NONE', #10261, #11112 ) ;
#2198 = DIRECTION ( 'NONE',  ( 0.000000000000000000, 0.000000000000000000, -1.000000000000000000 ) ) ;
#2199 = EDGE_CURVE ( 'NONE', #6983, #12059, #6012, .T. ) ;
#2200 = CARTESIAN_POINT ( 'NONE',  ( -1.960325907828584402, -2.849280167418937637, -0.1599823882018511501 ) ) ;
#2201 = DIRECTION ( 'NONE',  ( 0.000000000000000000, 0.000000000000000000, 1.000000000000000000 ) ) ;
#2202 = CIRCLE ( 'NONE', #4197, 0.01968503937007873641 ) ;
#2203 = CARTESIAN_POINT ( 'NONE',  ( -1.187879871879820026, 0.3305938048772318893, -0.05905511811023619190 ) ) ;
#2204 = ORIENTED_EDGE ( 'NONE', *, *, #7281, .F. ) ;
#2205 = FACE_OUTER_BOUND ( 'NONE', #5564, .T. ) ;
#2206 = LINE ( 'NONE', #13172, #7597 ) ;
#2207 = AXIS2_PLACEMENT_3D ( 'NONE', #6804, #13014, #3380 ) ;
#2208 = CARTESIAN_POINT ( 'NONE',  ( -0.05905511811023622659, 1.338582677165354395, -0.5952259495879738127 ) ) ;
#2209 = DIRECTION ( 'NONE',  ( -0.000000000000000000, -1.000000000000000000, -0.000000000000000000 ) ) ;
#2210 = VERTEX_POINT ( 'NONE', #7343 ) ;
#2211 = CARTESIAN_POINT ( 'NONE',  ( 0.000000000000000000, 2.165354330708661568, 0.000000000000000000 ) ) ;
#2212 = ORIENTED_EDGE ( 'NONE', *, *, #14769, .F. ) ;
#2213 = ORIENTED_EDGE ( 'NONE', *, *, #2047, .T. ) ;
#2214 = CIRCLE ( 'NONE', #10964, 0.003937007874015749712 ) ;
#2215 = SPHERICAL_SURFACE ( 'NONE', #1094, 0.003937007874015747977 ) ;
#2216 = DIRECTION ( 'NONE',  ( -0.5000000000000000000, -0.000000000000000000, -0.8660254037844388186 ) ) ;
#2217 = ADVANCED_FACE ( 'NONE', ( #12001 ), #1088, .T. ) ;
#2218 = DIRECTION ( 'NONE',  ( 0.8144815189573204606, -0.5801894994542525774, 1.283760644411384396E-16 ) ) ;
#2219 = CARTESIAN_POINT ( 'NONE',  ( 0.06692913385832208184, -0.2952755905511811330, -0.4190977005962941426 ) ) ;
#2220 = CYLINDRICAL_SURFACE ( 'NONE', #1940, 0.003937007874015724558 ) ;
#2221 = ADVANCED_FACE ( 'NONE', ( #1415 ), #12589, .T. ) ;
#2222 = FACE_OUTER_BOUND ( 'NONE', #5425, .T. ) ;
#2223 = EDGE_LOOP ( 'NONE', ( #6547, #14816, #3034, #4086 ) ) ;
#2224 = DIRECTION ( 'NONE',  ( -0.1408070410764336311, 0.9900370584898827708, 0.000000000000000000 ) ) ;
#2225 = DIRECTION ( 'NONE',  ( 1.000000000000000000, 0.000000000000000000, 3.614007241618347785E-16 ) ) ;
#2226 = CARTESIAN_POINT ( 'NONE',  ( -0.4591888763630546655, -0.4881889763779528324, 0.3787644491703233141 ) ) ;
#2227 = EDGE_CURVE ( 'NONE', #14454, #562, #14343, .T. ) ;
#2228 = LINE ( 'NONE', #15155, #15436 ) ;
#2229 = ORIENTED_EDGE ( 'NONE', *, *, #447, .F. ) ;
#2230 = VERTEX_POINT ( 'NONE', #9072 ) ;
#2231 = FACE_OUTER_BOUND ( 'NONE', #10129, .T. ) ;
#2232 = ORIENTED_EDGE ( 'NONE', *, *, #7982, .F. ) ;
#2233 = VERTEX_POINT ( 'NONE', #13708 ) ;
#2234 = EDGE_LOOP ( 'NONE', ( #13282, #1241, #11772 ) ) ;
#2235 = CYLINDRICAL_SURFACE ( 'NONE', #11137, 0.1771653543307079026 ) ;
#2236 = CARTESIAN_POINT ( 'NONE',  ( -0.06692913385815749128, -0.1023622047244094474, -0.2377126739438355507 ) ) ;
#2237 = DIRECTION ( 'NONE',  ( -1.000000000000000000, 0.000000000000000000, 0.000000000000000000 ) ) ;
#2238 = EDGE_CURVE ( 'NONE', #9448, #2526, #2885, .T. ) ;
#2239 = SHAPE_REPRESENTATION_RELATIONSHIP ( 'NONE' , 'NONE' ,  #2403, #3470 ) ;
#2240 = DIRECTION ( 'NONE',  ( -0.000000000000000000, -1.000000000000000000, -0.000000000000000000 ) ) ;
#2241 = EDGE_CURVE ( 'NONE', #13020, #13305, #5814, .T. ) ;
#2242 = DIRECTION ( 'NONE',  ( 1.000000000000000000, 0.000000000000000000, 0.000000000000000000 ) ) ;
#2243 = CARTESIAN_POINT ( 'NONE',  ( -1.391747264127679351, -0.02263456418309609669, 0.06141688777630970042 ) ) ;
#2244 = EDGE_CURVE ( 'NONE', #11495, #4530, #12100, .T. ) ;
#2245 = CARTESIAN_POINT ( 'NONE',  ( -1.398125690441303304, -0.003404927804347070153, -0.05905511811023622659 ) ) ;
#2246 = ORIENTED_EDGE ( 'NONE', *, *, #4659, .F. ) ;
#2247 = VERTEX_POINT ( 'NONE', #2797 ) ;
#2248 = ORIENTED_EDGE ( 'NONE', *, *, #10262, .F. ) ;
#2249 = ORIENTED_EDGE ( 'NONE', *, *, #15271, .T. ) ;
#2250 = CARTESIAN_POINT ( 'NONE',  ( 0.000000000000000000, -0.1023622047244094474, 0.1574803149606299191 ) ) ;
#2251 = EDGE_CURVE ( 'NONE', #10793, #11857, #830, .T. ) ;
#2252 = CARTESIAN_POINT ( 'NONE',  ( -0.002557446713253788174, 0.1765481709910070307, 0.0002437469044495125788 ) ) ;
#2253 = CARTESIAN_POINT ( 'NONE',  ( -0.5424655050177918936, 1.338877451511696570, 0.2450016286721715675 ) ) ;
#2254 = DIRECTION ( 'NONE',  ( 0.000000000000000000, -1.000000000000000000, -0.000000000000000000 ) ) ;
#2255 = DIRECTION ( 'NONE',  ( -0.000000000000000000, 0.000000000000000000, 1.000000000000000000 ) ) ;
#2256 = ORIENTED_EDGE ( 'NONE', *, *, #8742, .F. ) ;
#2257 =( CONVERSION_BASED_UNIT ( 'INCH', #69 ) LENGTH_UNIT ( ) NAMED_UNIT ( #4338 ) );
#2258 = EDGE_CURVE ( 'NONE', #12255, #241, #10092, .T. ) ;
#2259 = CARTESIAN_POINT ( 'NONE',  ( -0.1657884745773953172, -0.4881889763779528324, 0.2093696482190284536 ) ) ;
#2260 = CARTESIAN_POINT ( 'NONE',  ( -0.05175539059627463218, 0.06736074103232447818, 0.07475334604056275978 ) ) ;
#2261 = EDGE_CURVE ( 'NONE', #3506, #5709, #5462, .T. ) ;
#2262 = VERTEX_POINT ( 'NONE', #6483 ) ;
#2263 = VERTEX_POINT ( 'NONE', #11268 ) ;
#2264 = EDGE_CURVE ( 'NONE', #12221, #8322, #2579, .T. ) ;
#2265 = VERTEX_POINT ( 'NONE', #12898 ) ;
#2266 = CARTESIAN_POINT ( 'NONE',  ( -2.755905511811024056, -1.630597114118274238, -0.1033464566929129386 ) ) ;
#2267 = DIRECTION ( 'NONE',  ( -3.973232667114494807E-16, 0.000000000000000000, 1.000000000000000000 ) ) ;
#2268 = CARTESIAN_POINT ( 'NONE',  ( -0.5905511811023629321, -0.09448818897637796532, 0.1591122789105256785 ) ) ;
#2269 = CARTESIAN_POINT ( 'NONE',  ( 1.904470415996868375E-17, 2.165354330708661568, -0.1535433070866141780 ) ) ;
#2270 = CARTESIAN_POINT ( 'NONE',  ( -1.993155558009506167, -2.659219082276543578, 0.1643228695458794353 ) ) ;
#2271 = ORIENTED_EDGE ( 'NONE', *, *, #317, .F. ) ;
#2272 = CARTESIAN_POINT ( 'NONE',  ( 7.232166136696967594E-17, 2.433070866141732846, 0.5905511811023621549 ) ) ;
#2273 = FACE_OUTER_BOUND ( 'NONE', #2528, .T. ) ;
#2274 = DIRECTION ( 'NONE',  ( 0.8660254037844405950, -3.174764303743830077E-15, -0.4999999999999967248 ) ) ;
#2275 = CARTESIAN_POINT ( 'NONE',  ( -1.596293587998444563, 0.1133155780026525727, 0.04477369844320282927 ) ) ;
#2276 = EDGE_LOOP ( 'NONE', ( #15148, #7530, #11805, #12924 ) ) ;
#2277 = ORIENTED_EDGE ( 'NONE', *, *, #2035, .T. ) ;
#2278 = EDGE_CURVE ( 'NONE', #10886, #1546, #4139, .T. ) ;
#2279 = ORIENTED_EDGE ( 'NONE', *, *, #12012, .T. ) ;
#2280 = ORIENTED_EDGE ( 'NONE', *, *, #7586, .T. ) ;
#2281 = PRODUCT_DEFINITION_SHAPE ( 'NONE', 'NONE',  #15497 ) ;
#2282 = ORIENTED_EDGE ( 'NONE', *, *, #8759, .T. ) ;
#2283 = CARTESIAN_POINT ( 'NONE',  ( 0.000000000000000000, 1.338582677165354395, 0.000000000000000000 ) ) ;
#2284 = DIRECTION ( 'NONE',  ( 0.4999999999999966693, 0.000000000000000000, -0.8660254037844405950 ) ) ;
#2285 = DIRECTION ( 'NONE',  ( 0.000000000000000000, 0.000000000000000000, 1.000000000000000000 ) ) ;
#2286 = CARTESIAN_POINT ( 'NONE',  ( -0.2647411304678976007, -0.4881889763779528324, 0.03404161279859290595 ) ) ;
#2287 = CONTEXT_DEPENDENT_SHAPE_REPRESENTATION ( #9920, #2022 ) ;
#2288 = DIRECTION ( 'NONE',  ( -0.000000000000000000, -1.000000000000000000, -0.000000000000000000 ) ) ;
#2289 = CARTESIAN_POINT ( 'NONE',  ( -1.180847381051876699, 0.3433074774306786314, 0.04457071048068597663 ) ) ;
#2290 = ORIENTED_EDGE ( 'NONE', *, *, #11903, .T. ) ;
#2291 = DIRECTION ( 'NONE',  ( -0.000000000000000000, -1.000000000000000000, -0.000000000000000000 ) ) ;
#2292 = CARTESIAN_POINT ( 'NONE',  ( -2.755905511811024056, -2.749515453455444014, -0.1756903148397123138 ) ) ;
#2293 = DIRECTION ( 'NONE',  ( 0.4999999999999949485, 0.000000000000000000, -0.8660254037844415942 ) ) ;
#2294 = ORIENTED_EDGE ( 'NONE', *, *, #14633, .F. ) ;
#2295 = CARTESIAN_POINT ( 'NONE',  ( 0.09842519685044820443, -0.4881889763779528324, -0.5870514566507987197 ) ) ;
#2296 = ORIENTED_EDGE ( 'NONE', *, *, #11860, .F. ) ;
#2297 = ORIENTED_EDGE ( 'NONE', *, *, #15172, .T. ) ;
#2298 = EDGE_LOOP ( 'NONE', ( #2229, #3388, #1634, #14662 ) ) ;
#2299 = CARTESIAN_POINT ( 'NONE',  ( -1.985311755390326782, -2.772329397582949717, -0.1771653543307079026 ) ) ;
#2300 = EDGE_CURVE ( 'NONE', #8494, #8120, #93, .T. ) ;
#2301 = LINE ( 'NONE', #4885, #6328 ) ;
#2302 = CARTESIAN_POINT ( 'NONE',  ( -1.911369061871032837, -2.911955715286031143, -0.1096748193019170953 ) ) ;
#2303 = DIRECTION ( 'NONE',  ( 0.4999999999999930056, 0.000000000000000000, 0.8660254037844428154 ) ) ;
#2304 = CARTESIAN_POINT ( 'NONE',  ( -1.577626109319076653, 0.1055621384249483125, -0.06600777036499150263 ) ) ;
#2305 = FACE_OUTER_BOUND ( 'NONE', #13155, .T. ) ;
#2306 = DIRECTION ( 'NONE',  ( -1.224646799147358384E-16, 0.000000000000000000, -1.000000000000000000 ) ) ;
#2307 = FACE_OUTER_BOUND ( 'NONE', #13019, .T. ) ;
#2308 = ORIENTED_EDGE ( 'NONE', *, *, #4857, .T. ) ;
#2309 = ORIENTED_EDGE ( 'NONE', *, *, #12865, .F. ) ;
#2310 = ORIENTED_EDGE ( 'NONE', *, *, #15243, .F. ) ;
#2311 = EDGE_CURVE ( 'NONE', #4513, #13444, #2169, .T. ) ;
#2312 = VERTEX_POINT ( 'NONE', #5225 ) ;
#2313 = EDGE_CURVE ( 'NONE', #4716, #7918, #14093, .T. ) ;
#2314 = CARTESIAN_POINT ( 'NONE',  ( -1.574484809660005480, 0.1100025355994810050, -0.06175692796176410898 ) ) ;
#2315 = DIRECTION ( 'NONE',  ( 0.000000000000000000, 0.000000000000000000, 1.000000000000000000 ) ) ;
#2316 = CARTESIAN_POINT ( 'NONE',  ( -1.570515516786257892, 0.1150740656598345651, -0.05905511811023623353 ) ) ;
#2317 = CARTESIAN_POINT ( 'NONE',  ( -0.2681506793016946166, -0.1023622047244094474, 0.03207310886158502850 ) ) ;
#2318 = AXIS2_PLACEMENT_3D ( 'NONE', #6223, #5044, #9845 ) ;
#2319 = CARTESIAN_POINT ( 'NONE',  ( -0.3137366569588388998, -0.2952755905511811330, 0.2947875711430708590 ) ) ;
#2320 = ORIENTED_EDGE ( 'NONE', *, *, #4446, .F. ) ;
#2321 = SURFACE_STYLE_FILL_AREA ( #1249 ) ;
#2322 = VECTOR ( 'NONE', #11017, 39.37007874015748143 ) ;
#2323 = CARTESIAN_POINT ( 'NONE',  ( -0.2362204724409448231, -0.02638708502139245488, 0.05905511811023622659 ) ) ;
#2324 = CARTESIAN_POINT ( 'NONE',  ( -0.5379290338433416752, -0.1023622047244094474, 0.2423824958184911116 ) ) ;
#2325 = VECTOR ( 'NONE', #3957, 39.37007874015748143 ) ;
#2326 = ORIENTED_EDGE ( 'NONE', *, *, #359, .F. ) ;
#2327 = ADVANCED_FACE ( 'NONE', ( #6630 ), #7569, .F. ) ;
#2328 = EDGE_LOOP ( 'NONE', ( #12487, #9014, #13076, #9177 ) ) ;
#2329 = ADVANCED_FACE ( 'NONE', ( #1641 ), #6400, .F. ) ;
#2330 = ORIENTED_EDGE ( 'NONE', *, *, #11953, .F. ) ;
#2331 = AXIS2_PLACEMENT_3D ( 'NONE', #3037, #12593, #1861 ) ;
#2332 = AXIS2_PLACEMENT_3D ( 'NONE', #4036, #686, #11080 ) ;
#2333 = CARTESIAN_POINT ( 'NONE',  ( -1.990041431622598944, -2.757151776041542046, 0.1766819155262782659 ) ) ;
#2334 = CIRCLE ( 'NONE', #11601, 0.2165354330708662012 ) ;
#2335 = EDGE_CURVE ( 'NONE', #3128, #6177, #4588, .T. ) ;
#2336 = CIRCLE ( 'NONE', #8853, 0.5905511811023621549 ) ;
#2337 = CARTESIAN_POINT ( 'NONE',  ( -1.953876537811547465, -2.911231419079650440, -0.08677724235065008285 ) ) ;
#2338 = LINE ( 'NONE', #12061, #10622 ) ;
#2339 = CARTESIAN_POINT ( 'NONE',  ( -1.956881466196074948, -2.859458241652981680, 0.1546921351859912863 ) ) ;
#2340 = DIRECTION ( 'NONE',  ( 0.000000000000000000, 0.000000000000000000, 1.000000000000000000 ) ) ;
#2341 = CARTESIAN_POINT ( 'NONE',  ( -1.181342415307386151, 0.3435647566351286430, -0.04453711288980863325 ) ) ;
#2342 = ORIENTED_EDGE ( 'NONE', *, *, #1659, .F. ) ;
#2343 = CARTESIAN_POINT ( 'NONE',  ( -1.943213732889473411, -2.937317281408696523, -0.01189756183868651701 ) ) ;
#2344 = CARTESIAN_POINT ( 'NONE',  ( -0.06438893898759806556, 1.344775570699244582, -0.5870328364109891339 ) ) ;
#2345 = VECTOR ( 'NONE', #12663, 39.37007874015748143 ) ;
#2346 = CARTESIAN_POINT ( 'NONE',  ( 0.5405798186813290940, 1.344775570699301648, 0.2377539613195566448 ) ) ;
#2347 = CARTESIAN_POINT ( 'NONE',  ( -0.05905511811012585655, -0.1023622047244094474, -0.5909884645248143498 ) ) ;
#2348 = ORIENTED_EDGE ( 'NONE', *, *, #13177, .F. ) ;
#2349 = CIRCLE ( 'NONE', #8114, 1.865354330708661745 ) ;
#2350 = CIRCLE ( 'NONE', #13608, 0.007874015748031516770 ) ;
#2351 = AXIS2_PLACEMENT_3D ( 'NONE', #740, #9111, #12492 ) ;
#2352 = ORIENTED_EDGE ( 'NONE', *, *, #10559, .F. ) ;
#2353 = EDGE_LOOP ( 'NONE', ( #13730, #3537, #6665 ) ) ;
#2354 = CARTESIAN_POINT ( 'NONE',  ( 0.1022864650139100745, 0.000000000000000000, 1.563012696487738457E-17 ) ) ;
#2355 = EDGE_CURVE ( 'NONE', #4854, #6320, #13344, .T. ) ;
#2356 = DIRECTION ( 'NONE',  ( 0.000000000000000000, 0.000000000000000000, -1.000000000000000000 ) ) ;
#2357 = AXIS2_PLACEMENT_3D ( 'NONE', #9664, #1339, #1274 ) ;
#2358 = AXIS2_PLACEMENT_3D ( 'NONE', #12701, #11762, #10566 ) ;
#2359 = VECTOR ( 'NONE', #9410, 39.37007874015748143 ) ;
#2360 = CARTESIAN_POINT ( 'NONE',  ( -1.603601197326160355, 0.1030128816188568691, -0.05620285841715500635 ) ) ;
#2361 = CARTESIAN_POINT ( 'NONE',  ( -0.05905511811023622659, 1.043307086614173373, -0.5955041639236610118 ) ) ;
#2362 = CARTESIAN_POINT ( 'NONE',  ( -0.09842519685028340570, -0.1023622047244094474, -0.5870514566507987197 ) ) ;
#2363 = AXIS2_PLACEMENT_3D ( 'NONE', #10903, #7520, #7289 ) ;
#2364 = FACE_OUTER_BOUND ( 'NONE', #11745, .T. ) ;
#2365 = EDGE_CURVE ( 'NONE', #161, #13241, #9085, .T. ) ;
#2367 = VERTEX_POINT ( 'NONE', #6868 ) ;
#2366 = AXIS2_PLACEMENT_3D ( 'NONE', #1227, #13429, #7470 ) ;
#2368 = DIRECTION ( 'NONE',  ( 1.000000000000000000, 0.000000000000000000, 0.000000000000000000 ) ) ;
#2369 = EDGE_CURVE ( 'NONE', #6293, #13266, #15343, .T. ) ;
#2370 = CARTESIAN_POINT ( 'NONE',  ( 0.5629921259842255443, -0.4881889763779528324, 0.2068459625837324456 ) ) ;
#2371 = SURFACE_STYLE_USAGE ( .BOTH. , #9202 ) ;
#2372 = FACE_OUTER_BOUND ( 'NONE', #13231, .T. ) ;
#2373 = VECTOR ( 'NONE', #13666, 39.37007874015748143 ) ;
#2374 = AXIS2_PLACEMENT_3D ( 'NONE', #4256, #8891, #13670 ) ;
#2375 = AXIS2_PLACEMENT_3D ( 'NONE', #6022, #4944, #5958 ) ;
#2376 = ORIENTED_EDGE ( 'NONE', *, *, #11462, .F. ) ;
#2377 = ORIENTED_EDGE ( 'NONE', *, *, #3447, .T. ) ;
#2378 = VERTEX_POINT ( 'NONE', #3562 ) ;
#2379 = AXIS2_PLACEMENT_3D ( 'NONE', #7897, #6304, #11101 ) ;
#2380 = ORIENTED_EDGE ( 'NONE', *, *, #4251, .F. ) ;
#2381 = ORIENTED_EDGE ( 'NONE', *, *, #14521, .T. ) ;
#2382 = ORIENTED_EDGE ( 'NONE', *, *, #10303, .T. ) ;
#2383 = CARTESIAN_POINT ( 'NONE',  ( 0.06299212598430636856, -0.2952755905511811330, -0.4190977005962941426 ) ) ;
#2384 = DIRECTION ( 'NONE',  ( -0.5000000000000004441, 0.000000000000000000, 0.8660254037844384856 ) ) ;
#2385 = CARTESIAN_POINT ( 'NONE',  ( 0.4121618538092042816, -0.2952755905511811330, 0.1243101294532687889 ) ) ;
#2386 = DIRECTION ( 'NONE',  ( -1.110223024625156294E-16, 0.5030755238499721171, 0.8642424528470445955 ) ) ;
#2387 = AXIS2_PLACEMENT_3D ( 'NONE', #11988, #154, #1173 ) ;
#2388 = DIRECTION ( 'NONE',  ( -0.8660254037844427044, 0.000000000000000000, 0.4999999999999929501 ) ) ;
#2389 = CIRCLE ( 'NONE', #395, 0.007874015748031482076 ) ;
#2390 = CIRCLE ( 'NONE', #397, 0.04330708661417331101 ) ;
#2391 = CARTESIAN_POINT ( 'NONE',  ( 0.4815353412745612127, 0.000000000000000000, 0.3552976658085785222 ) ) ;
#2392 = CARTESIAN_POINT ( 'NONE',  ( -1.591501945092674175, 0.08600752902535276079, 0.1033464566929133410 ) ) ;
#2393 = CARTESIAN_POINT ( 'NONE',  ( -0.5860051159906336515, -0.003937007874015747977, 0.1591122789105256785 ) ) ;
#2394 = TOROIDAL_SURFACE ( 'NONE', #5895, 0.05905511811023614333, 0.01968503937007873988 ) ;
#2395 = FACE_OUTER_BOUND ( 'NONE', #9903, .T. ) ;
#2396 = ORIENTED_EDGE ( 'NONE', *, *, #422, .F. ) ;
#2397 = ORIENTED_EDGE ( 'NONE', *, *, #1089, .F. ) ;
#2398 = VECTOR ( 'NONE', #689, 39.37007874015748143 ) ;
#2399 = ORIENTED_EDGE ( 'NONE', *, *, #13951, .T. ) ;
#2400 = AXIS2_PLACEMENT_3D ( 'NONE', #14720, #13375, #9711 ) ;
#2401 = VECTOR ( 'NONE', #12556, 39.37007874015748143 ) ;
#2402 = VERTEX_POINT ( 'NONE', #1297 ) ;
#2403 = SHAPE_REPRESENTATION ( 'Nut', ( #11481 ), #7714 ) ;
#2404 = AXIS2_PLACEMENT_3D ( 'NONE', #5565, #1050, #4649 ) ;
#2405 = B_SPLINE_CURVE_WITH_KNOTS ( 'NONE', 3,
 ( #180, #2346, #4939, #4780, #7131, #14338 ),
 .UNSPECIFIED., .F., .F.,
 ( 4, 2, 4 ),
 ( -2.828444569872989946E-06, 0.0001777364543001158713, 0.0003583013531701047033 ),
 .UNSPECIFIED. ) ;
#2406 = CARTESIAN_POINT ( 'NONE',  ( -2.104378391724875286, -1.678230452895279612, -0.1033464566929128969 ) ) ;
#2407 = DIRECTION ( 'NONE',  ( -1.000000000000000000, -0.000000000000000000, -0.000000000000000000 ) ) ;
#2408 = EDGE_CURVE ( 'NONE', #2265, #624, #7824, .T. ) ;
#2409 = FACE_OUTER_BOUND ( 'NONE', #1037, .T. ) ;
#2410 = DIRECTION ( 'NONE',  ( 0.000000000000000000, -1.000000000000000000, 0.000000000000000000 ) ) ;
#2411 = AXIS2_PLACEMENT_3D ( 'NONE', #285, #12041, #7314 ) ;
#2412 = PLANE ( 'NONE',  #2387 ) ;
#2413 = ADVANCED_FACE ( 'NONE', ( #12979 ), #3587, .T. ) ;
#2414 = ORIENTED_EDGE ( 'NONE', *, *, #13531, .F. ) ;
#2415 = DIRECTION ( 'NONE',  ( 0.5000000000000069944, 0.000000000000000000, -0.8660254037844347108 ) ) ;
#2416 = CARTESIAN_POINT ( 'NONE',  ( 0.1062992125984796865, -0.1023622047244094474, -0.5870514566507987197 ) ) ;
#2417 = CARTESIAN_POINT ( 'NONE',  ( 0.000000000000000000, 0.5433070866141731514, 0.6614173228346456046 ) ) ;
#2418 = AXIS2_PLACEMENT_3D ( 'NONE', #8799, #510, #7854 ) ;
#2419 = ORIENTED_EDGE ( 'NONE', *, *, #454, .F. ) ;
#2420 = EDGE_CURVE ( 'NONE', #9440, #14646, #14588, .T. ) ;
#2421 = VERTEX_POINT ( 'NONE', #11802 ) ;
#2422 = VERTEX_POINT ( 'NONE', #4894 ) ;
#2423 = AXIS2_PLACEMENT_3D ( 'NONE', #3713, #10758, #9676 ) ;
#2424 = LINE ( 'NONE', #1183, #9399 ) ;
#2425 = VECTOR ( 'NONE', #14502, 39.37007874015748143 ) ;
#2426 = EDGE_CURVE ( 'NONE', #5050, #2901, #10925, .T. ) ;
#2427 = CARTESIAN_POINT ( 'NONE',  ( -0.1181102362204724254, 2.448818897637795367, -0.03937007874015747977 ) ) ;
#2428 = CARTESIAN_POINT ( 'NONE',  ( -0.5412721729274213578, 1.041728495490239492, 0.2430720373988195515 ) ) ;
#2429 = CARTESIAN_POINT ( 'NONE',  ( -2.073793831555243550, -2.576344762740146788, 0.1326668340823329850 ) ) ;
#2430 = LINE ( 'NONE', #7209, #3692 ) ;
#2431 = CARTESIAN_POINT ( 'NONE',  ( -1.181342415325283612, 0.3435647566447525558, -0.03937007874014958331 ) ) ;
#2432 = EDGE_CURVE ( 'NONE', #851, #15395, #8427, .T. ) ;
#2433 = ORIENTED_EDGE ( 'NONE', *, *, #9553, .F. ) ;
#2434 = CARTESIAN_POINT ( 'NONE',  ( -2.010991777528384983, -2.758467574604075434, 0.1561691687464104861 ) ) ;
#2435 = DIRECTION ( 'NONE',  ( -0.8660254037844385966, 0.000000000000000000, -0.5000000000000002220 ) ) ;
#2436 = AXIS2_PLACEMENT_3D ( 'NONE', #4997, #12369, #8608 ) ;
#2437 = AXIS2_PLACEMENT_3D ( 'NONE', #14034, #1979, #965 ) ;
#2438 = PLANE ( 'NONE',  #11723 ) ;
#2439 = VERTEX_POINT ( 'NONE', #2392 ) ;
#2440 = EDGE_CURVE ( 'NONE', #11092, #10823, #13580, .T. ) ;
#2441 = ADVANCED_FACE ( 'NONE', ( #10771 ), #5061, .T. ) ;
#2442 = AXIS2_PLACEMENT_3D ( 'NONE', #2188, #4525, #9308 ) ;
#2443 = AXIS2_PLACEMENT_3D ( 'NONE', #12707, #12475, #6729 ) ;
#2444 = ORIENTED_EDGE ( 'NONE', *, *, #14260, .F. ) ;
#2445 = CYLINDRICAL_SURFACE ( 'NONE', #11895, 0.003937007874015737569 ) ;
#2446 = CARTESIAN_POINT ( 'NONE',  ( -0.05114323250695500950, 0.05905511811023622659, 0.08858267716535433989 ) ) ;
#2447 = CIRCLE ( 'NONE', #11201, 0.003937007874015749712 ) ;
#2448 = CARTESIAN_POINT ( 'NONE',  ( -1.419113452591957980, -0.01195610050880212445, 0.07344571687920077585 ) ) ;
#2449 = CARTESIAN_POINT ( 'NONE',  ( 0.5413385826772204590, -0.1023622047244094474, 0.2443509997555466662 ) ) ;
#2450 = CARTESIAN_POINT ( 'NONE',  ( 0.09842519685044820443, -0.4921259842519685179, -0.5870514566507987197 ) ) ;
#2451 = CIRCLE ( 'NONE', #4942, 0.003937007874015754916 ) ;
#2452 = DIRECTION ( 'NONE',  ( 0.5000000000000035527, 0.000000000000000000, -0.8660254037844365982 ) ) ;
#2453 = CARTESIAN_POINT ( 'NONE',  ( 1.181102362204724310, 4.044111181948214319E-16, -0.02952755905511811330 ) ) ;
#2454 = VERTEX_POINT ( 'NONE', #5113 ) ;
#2455 = FACE_OUTER_BOUND ( 'NONE', #13676, .T. ) ;
#2456 = FACE_OUTER_BOUND ( 'NONE', #8094, .T. ) ;
#2457 = CARTESIAN_POINT ( 'NONE',  ( -0.07874015748031543138, -0.1682792322177920907, 0.05905511811023622659 ) ) ;
#2458 = EDGE_CURVE ( 'NONE', #8212, #13463, #7079, .T. ) ;
#2459 = SURFACE_SIDE_STYLE ('',( #13194 ) ) ;
#2460 = EDGE_CURVE ( 'NONE', #7138, #13559, #8800, .T. ) ;
#2461 = AXIS2_PLACEMENT_3D ( 'NONE', #6327, #12247, #11042 ) ;
#2462 = ORIENTED_EDGE ( 'NONE', *, *, #8039, .F. ) ;
#2463 = ORIENTED_EDGE ( 'NONE', *, *, #10759, .T. ) ;
#2464 = VERTEX_POINT ( 'NONE', #8890 ) ;
#2465 = CIRCLE ( 'NONE', #11210, 0.003937007874015750579 ) ;
#2466 = ORIENTED_EDGE ( 'NONE', *, *, #428, .T. ) ;
#2467 = EDGE_CURVE ( 'NONE', #6881, #1627, #11074, .T. ) ;
#2468 = DIRECTION ( 'NONE',  ( 0.4999999999999966693, 0.000000000000000000, -0.8660254037844405950 ) ) ;
#2469 = PLANE ( 'NONE',  #8600 ) ;
#2470 = CARTESIAN_POINT ( 'NONE',  ( -1.953792993931855904, -2.783665366331675273, -0.1771653543307734335 ) ) ;
#2471 = CARTESIAN_POINT ( 'NONE',  ( 0.3117681530247254362, 35.52269057326157053, 0.2981971199779697157 ) ) ;
#2472 = AXIS2_PLACEMENT_3D ( 'NONE', #6545, #11340, #11429 ) ;
#2473 = LINE ( 'NONE', #5983, #13602 ) ;
#2474 = CARTESIAN_POINT ( 'NONE',  ( -0.1023622047242992716, -0.1023622047244094474, -0.2482618547482104143 ) ) ;
#2475 = DIRECTION ( 'NONE',  ( 0.000000000000000000, 1.000000000000000000, 0.000000000000000000 ) ) ;
#2476 = CARTESIAN_POINT ( 'NONE',  ( 0.2681506793018588186, -0.4921259842519685179, 0.03207310886168001501 ) ) ;
#2477 = CARTESIAN_POINT ( 'NONE',  ( 0.05905511811023622659, 1.043307086614173373, -0.5511811023622047445 ) ) ;
#2478 = EDGE_LOOP ( 'NONE', ( #14334, #10168, #15041, #24 ) ) ;
#2479 = ORIENTED_EDGE ( 'NONE', *, *, #4908, .F. ) ;
#2480 = ORIENTED_EDGE ( 'NONE', *, *, #8707, .F. ) ;
#2481 = ADVANCED_FACE ( 'NONE', ( #9829 ), #12855, .T. ) ;
#2482 = DIRECTION ( 'NONE',  ( -1.000000000000000000, -0.000000000000000000, -0.000000000000000000 ) ) ;
#2483 = DIRECTION ( 'NONE',  ( -0.000000000000000000, 1.000000000000000000, -0.000000000000000000 ) ) ;
#2484 = DIRECTION ( 'NONE',  ( 0.000000000000000000, -0.000000000000000000, -1.000000000000000000 ) ) ;
#2485 = CARTESIAN_POINT ( 'NONE',  ( 0.1552072824047652233, -0.09448818897637796532, -0.5870514566507987197 ) ) ;
#2486 = DIRECTION ( 'NONE',  ( -0.000000000000000000, 0.000000000000000000, 1.000000000000000000 ) ) ;
#2487 = CARTESIAN_POINT ( 'NONE',  ( -0.1586168312385622670, -0.09842519685039370636, -0.5890199605878064792 ) ) ;
#2488 = DIRECTION ( 'NONE',  ( 0.000000000000000000, 0.000000000000000000, 1.000000000000000000 ) ) ;
#2489 = DIRECTION ( 'NONE',  ( 0.000000000000000000, 0.000000000000000000, 1.000000000000000000 ) ) ;
#2490 = ORIENTED_EDGE ( 'NONE', *, *, #2629, .F. ) ;
#2491 = ORIENTED_EDGE ( 'NONE', *, *, #14633, .T. ) ;
#2492 = EDGE_LOOP ( 'NONE', ( #11115, #12466, #12355, #2600 ) ) ;
#2493 = EDGE_CURVE ( 'NONE', #9186, #12161, #8734, .T. ) ;
#2494 = DIRECTION ( 'NONE',  ( -0.000000000000000000, 1.000000000000000000, -0.000000000000000000 ) ) ;
#2495 = CARTESIAN_POINT ( 'NONE',  ( -1.577626107947794232, 0.1055621403655416374, 0.06600776443432196383 ) ) ;
#2496 = ADVANCED_FACE ( 'NONE', ( #1457 ), #9607, .T. ) ;
#2497 = DIRECTION ( 'NONE',  ( 0.000000000000000000, 0.000000000000000000, -1.000000000000000000 ) ) ;
#2498 = DIRECTION ( 'NONE',  ( 0.000000000000000000, 0.000000000000000000, 1.000000000000000000 ) ) ;
#2499 = DIRECTION ( 'NONE',  ( 0.4999999999999920064, 0.000000000000000000, -0.8660254037844433705 ) ) ;
#2500 = DIRECTION ( 'NONE',  ( 0.000000000000000000, 1.000000000000000000, 0.000000000000000000 ) ) ;
#2501 = CARTESIAN_POINT ( 'NONE',  ( -1.180847381051816525, 0.3433074774307514065, -0.03937007874014958331 ) ) ;
#2502 = ORIENTED_EDGE ( 'NONE', *, *, #15099, .T. ) ;
#2503 = DIRECTION ( 'NONE',  ( 1.000000000000000000, 0.000000000000000000, 0.000000000000000000 ) ) ;
#2504 = CARTESIAN_POINT ( 'NONE',  ( 0.000000000000000000, 0.000000000000000000, 0.000000000000000000 ) ) ;
#2505 = ORIENTED_EDGE ( 'NONE', *, *, #513, .T. ) ;
#2506 = VERTEX_POINT ( 'NONE', #13570 ) ;
#2507 = ADVANCED_FACE ( 'NONE', ( #5258 ), #6444, .T. ) ;
#2508 = UNCERTAINTY_MEASURE_WITH_UNIT (LENGTH_MEASURE( 1.000000000000000082E-05 ), #2686, 'distance_accuracy_value', 'NONE');
#2509 = ORIENTED_EDGE ( 'NONE', *, *, #13243, .T. ) ;
#2510 = ADVANCED_FACE ( 'NONE', ( #11154, #7397 ), #3795, .F. ) ;
#2511 = DIRECTION ( 'NONE',  ( 0.4999999999999981681, -0.000000000000000000, 0.8660254037844397068 ) ) ;
#2512 = CARTESIAN_POINT ( 'NONE',  ( -0.4586614173228359959, -0.09448818897637796532, 0.3875520507749251053 ) ) ;
#2513 = EDGE_CURVE ( 'NONE', #9857, #13620, #9852, .T. ) ;
#2514 = CARTESIAN_POINT ( 'NONE',  ( -0.06604848736013260724, 1.035433070866141891, -0.5868460571724354313 ) ) ;
#2515 = FACE_OUTER_BOUND ( 'NONE', #2899, .T. ) ;
#2516 = ITEM_DEFINED_TRANSFORMATION ( 'NONE', 'NONE', #2366,  #11481 ) ;
#2517 = DIRECTION ( 'NONE',  ( 0.000000000000000000, 0.000000000000000000, 1.000000000000000000 ) ) ;
#2518 = CARTESIAN_POINT ( 'NONE',  ( -0.02641567992992046449, 0.1724028871747071145, 1.853431881210122409E-17 ) ) ;
#2519 = ORIENTED_EDGE ( 'NONE', *, *, #8122, .F. ) ;
#2520 = CARTESIAN_POINT ( 'NONE',  ( -1.577626107947872613, 0.1055621403655540441, -0.06600776443437042507 ) ) ;
#2521 = CARTESIAN_POINT ( 'NONE',  ( 0.000000000000000000, 0.3464566929133857109, 0.000000000000000000 ) ) ;
#2522 = CARTESIAN_POINT ( 'NONE',  ( 0.000000000000000000, 0.4133858267716535306, 0.03543307086614173179 ) ) ;
#2523 = DIRECTION ( 'NONE',  ( 0.000000000000000000, 0.000000000000000000, -1.000000000000000000 ) ) ;
#2524 = ORIENTED_EDGE ( 'NONE', *, *, #15389, .F. ) ;
#2525 = VERTEX_POINT ( 'NONE', #7710 ) ;
#2526 = VERTEX_POINT ( 'NONE', #7623 ) ;
#2527 = ADVANCED_FACE ( 'NONE', ( #6512 ), #15101, .F. ) ;
#2528 = EDGE_LOOP ( 'NONE', ( #8776, #9819, #15272, #2131 ) ) ;
#2529 = DIRECTION ( 'NONE',  ( 0.8660254037844385966, 0.000000000000000000, 0.5000000000000001110 ) ) ;
#2530 = EDGE_CURVE ( 'NONE', #11605, #13986, #11065, .T. ) ;
#2531 = CARTESIAN_POINT ( 'NONE',  ( -0.09842519685028337795, -0.2952755905511811330, -0.3797276218561366767 ) ) ;
#2532 = DIRECTION ( 'NONE',  ( -0.000000000000000000, 1.000000000000000000, 0.000000000000000000 ) ) ;
#2533 = DIRECTION ( 'NONE',  ( -0.1305055777265677897, 0.9885803249658943193, -0.07534743043118216632 ) ) ;
#2534 = DIRECTION ( 'NONE',  ( 0.000000000000000000, -0.000000000000000000, -1.000000000000000000 ) ) ;
#2535 = CARTESIAN_POINT ( 'NONE',  ( -0.08151194962748883888, 0.1637246173173400876, 0.03937007874015747977 ) ) ;
#2536 = FACE_OUTER_BOUND ( 'NONE', #9451, .T. ) ;
#2537 = CYLINDRICAL_SURFACE ( 'NONE', #6861, 0.003937007874015757518 ) ;
#2538 = EDGE_CURVE ( 'NONE', #4047, #9540, #13979, .T. ) ;
#2539 = DIRECTION ( 'NONE',  ( -0.000000000000000000, -1.000000000000000000, -0.000000000000000000 ) ) ;
#2540 = CARTESIAN_POINT ( 'NONE',  ( 0.1181102362204724254, 2.448818897637795367, 0.03937007874015747977 ) ) ;
#2541 = ORIENTED_EDGE ( 'NONE', *, *, #8873, .T. ) ;
#2542 = ORIENTED_EDGE ( 'NONE', *, *, #151, .F. ) ;
#2543 = VERTEX_POINT ( 'NONE', #3167 ) ;
#2544 = LINE ( 'NONE', #12045, #8352 ) ;
#2545 = FACE_OUTER_BOUND ( 'NONE', #3111, .T. ) ;
#2546 = ADVANCED_FACE ( 'NONE', ( #7943 ), #4839, .T. ) ;
#2547 = FACE_OUTER_BOUND ( 'NONE', #2787, .T. ) ;
#2548 = CARTESIAN_POINT ( 'NONE',  ( 0.000000000000000000, 0.03937007874015749365, -0.1653543307086614012 ) ) ;
#2549 = LINE ( 'NONE', #371, #9330 ) ;
#2550 = CARTESIAN_POINT ( 'NONE',  ( 4.821444091131311524E-18, 0.1692468441617604180, 0.03937007874015747977 ) ) ;
#2551 = EDGE_CURVE ( 'NONE', #11565, #8556, #3091, .T. ) ;
#2552 = CARTESIAN_POINT ( 'NONE',  ( -0.1062992125983148878, -0.09842519685039370636, -0.5870514566507987197 ) ) ;
#2553 = ADVANCED_FACE ( 'NONE', ( #14929 ), #11861, .T. ) ;
#2554 = DIRECTION ( 'NONE',  ( 0.5163221703362063097, 0.6912615786716231892, 0.5055381748906061512 ) ) ;
#2555 = CARTESIAN_POINT ( 'NONE',  ( 0.4857119623810668974, 1.043292445042268257, 0.3486169089052639780 ) ) ;
#2556 = ORIENTED_EDGE ( 'NONE', *, *, #4159, .F. ) ;
#2557 = EDGE_LOOP ( 'NONE', ( #3590, #7197 ) ) ;
#2558 = ORIENTED_EDGE ( 'NONE', *, *, #11812, .T. ) ;
#2559 = VERTEX_POINT ( 'NONE', #13749 ) ;
#2560 = CARTESIAN_POINT ( 'NONE',  ( -2.099922416332451913, -2.385393657770973785, 0.1341751375602837637 ) ) ;
#2561 = CARTESIAN_POINT ( 'NONE',  ( 0.4141303577462121521, -0.2952755905511811330, 0.1209005806194717869 ) ) ;
#2562 = CIRCLE ( 'NONE', #5302, 0.007874015748031449116 ) ;
#2563 = VECTOR ( 'NONE', #14637, 39.37007874015748143 ) ;
#2564 = LINE ( 'NONE', #4993, #10853 ) ;
#2565 = LINE ( 'NONE', #12147, #7890 ) ;
#2566 = CARTESIAN_POINT ( 'NONE',  ( -2.182693454834260027, -1.630005269948474389, 0.08366141732283427501 ) ) ;
#2567 = CARTESIAN_POINT ( 'NONE',  ( 0.03357817649489055339, -0.2952755905511811330, 0.7012961359976183084 ) ) ;
#2568 = CARTESIAN_POINT ( 'NONE',  ( -1.898433237323783107, -2.875582490238674183, 0.1128268272022943663 ) ) ;
#2569 = ORIENTED_EDGE ( 'NONE', *, *, #8368, .T. ) ;
#2570 = CYLINDRICAL_SURFACE ( 'NONE', #8198, 0.03937007874015759773 ) ;
#2571 = PRODUCT_RELATED_PRODUCT_CATEGORY ( 'part', '', ( #8027 ) ) ;
#2572 = DIRECTION ( 'NONE',  ( 0.000000000000000000, -1.000000000000000000, 0.000000000000000000 ) ) ;
#2573 = DIRECTION ( 'NONE',  ( -1.000000000000000000, 0.000000000000000000, 0.000000000000000000 ) ) ;
#2574 = VERTEX_POINT ( 'NONE', #6589 ) ;
#2575 = ORIENTED_EDGE ( 'NONE', *, *, #12774, .F. ) ;
#2576 = AXIS2_PLACEMENT_3D ( 'NONE', #1945, #7970, #12820 ) ;
#2577 = VECTOR ( 'NONE', #7488, 39.37007874015748854 ) ;
#2578 = AXIS2_PLACEMENT_3D ( 'NONE', #6052, #6427, #1744 ) ;
#2579 = CIRCLE ( 'NONE', #3336, 0.04330708661417324162 ) ;
#2580 = ORIENTED_EDGE ( 'NONE', *, *, #10746, .F. ) ;
#2581 = CARTESIAN_POINT ( 'NONE',  ( -0.1062992125983148878, -0.09448818897637796532, -0.5909884645248143498 ) ) ;
#2582 = CARTESIAN_POINT ( 'NONE',  ( -1.605562881068252512, 0.1002320922365774053, -0.06209859025001985416 ) ) ;
#2583 = CARTESIAN_POINT ( 'NONE',  ( 0.09842519685044796851, -0.4921259842519685179, 3.910662073933746312E-17 ) ) ;
#2584 = ITEM_DEFINED_TRANSFORMATION ( 'NONE', 'NONE', #9882,  #11481 ) ;
#2585 = DIRECTION ( 'NONE',  ( -0.8660254037844347108, 0.000000000000000000, -0.5000000000000069944 ) ) ;
#2586 = DIRECTION ( 'NONE',  ( 0.000000000000000000, 0.000000000000000000, -1.000000000000000000 ) ) ;
#2587 = AXIS2_PLACEMENT_3D ( 'NONE', #15225, #8078, #11470 ) ;
#2588 = DIRECTION ( 'NONE',  ( 0.8660254037844249408, 0.000000000000000000, -0.5000000000000236478 ) ) ;
#2589 = ORIENTED_EDGE ( 'NONE', *, *, #4787, .F. ) ;
#2590 = FACE_BOUND ( 'NONE', #7749, .T. ) ;
#2591 = PRESENTATION_LAYER_ASSIGNMENT (  '', '', ( #1360 ) ) ;
#2592 = DIRECTION ( 'NONE',  ( 0.8660254037844385966, 0.000000000000000000, 0.5000000000000000000 ) ) ;
#2593 = VECTOR ( 'NONE', #14677, 39.37007874015748143 ) ;
#2594 = DIRECTION ( 'NONE',  ( -0.8660254037844390407, 0.000000000000000000, 0.4999999999999994449 ) ) ;
#2595 = DIRECTION ( 'NONE',  ( -0.000000000000000000, -1.000000000000000000, -0.000000000000000000 ) ) ;
#2596 = EDGE_CURVE ( 'NONE', #8551, #8, #14356, .T. ) ;
#2597 = SURFACE_STYLE_USAGE ( .BOTH. , #2459 ) ;
#2598 = ORIENTED_EDGE ( 'NONE', *, *, #9520, .F. ) ;
#2599 = EDGE_CURVE ( 'NONE', #14001, #12118, #9363, .T. ) ;
#2600 = ORIENTED_EDGE ( 'NONE', *, *, #5754, .T. ) ;
#2602 = ORIENTED_EDGE ( 'NONE', *, *, #1707, .F. ) ;
#2601 = VECTOR ( 'NONE', #10769, 39.37007874015748143 ) ;
#2603 = AXIS2_PLACEMENT_3D ( 'NONE', #15323, #5911, #6768 ) ;
#2604 = EDGE_LOOP ( 'NONE', ( #7424, #14538, #9077, #7840 ) ) ;
#2605 = CIRCLE ( 'NONE', #12123, 0.003937007874015724558 ) ;
#2606 = TOROIDAL_SURFACE ( 'NONE', #14627, 0.05905511811023614333, 0.01968503937007873988 ) ;
#2607 = VECTOR ( 'NONE', #10557, 39.37007874015748143 ) ;
#2608 = DIRECTION ( 'NONE',  ( -1.000000000000000000, 0.000000000000000000, 0.000000000000000000 ) ) ;
#2609 = AXIS2_PLACEMENT_3D ( 'NONE', #14208, #5794, #3477 ) ;
#2610 = AXIS2_PLACEMENT_3D ( 'NONE', #7547, #12643, #13565 ) ;
#2611 = DIRECTION ( 'NONE',  ( 1.000000000000000000, -0.000000000000000000, -0.000000000000000000 ) ) ;
#2612 = DIRECTION ( 'NONE',  ( 0.000000000000000000, 0.000000000000000000, 1.000000000000000000 ) ) ;
#2613 = CARTESIAN_POINT ( 'NONE',  ( -0.4141303577462325247, 35.52269057325969470, 0.1209005806194876492 ) ) ;
#2614 = DIRECTION ( 'NONE',  ( -0.000000000000000000, -1.000000000000000000, -0.000000000000000000 ) ) ;
#2615 = CARTESIAN_POINT ( 'NONE',  ( -0.05809364415030899426, 0.1671978997630558517, 0.03476146466084937409 ) ) ;
#2616 = EDGE_CURVE ( 'NONE', #3033, #9504, #7091, .T. ) ;
#2617 = CARTESIAN_POINT ( 'NONE',  ( -0.4783464566929145900, -0.4921259842519685179, 0.3534565624369550574 ) ) ;
#2618 = CARTESIAN_POINT ( 'NONE',  ( 0.000000000000000000, 1.661417322834646049, 0.000000000000000000 ) ) ;
#2619 = DIRECTION ( 'NONE',  ( -1.060575238724906792E-16, 1.000000000000000000, -6.123233995736767268E-17 ) ) ;
#2620 = VECTOR ( 'NONE', #6510, 39.37007874015748854 ) ;
#2621 = CIRCLE ( 'NONE', #4862, 0.003937007874015745375 ) ;
#2622 = AXIS2_PLACEMENT_3D ( 'NONE', #3403, #10689, #15386 ) ;
#2623 = EDGE_CURVE ( 'NONE', #11872, #12443, #8603, .T. ) ;
#2624 = AXIS2_PLACEMENT_3D ( 'NONE', #3618, #7285, #1271 ) ;
#2625 = DIRECTION ( 'NONE',  ( 0.000000000000000000, 1.000000000000000000, 0.000000000000000000 ) ) ;
#2626 = CARTESIAN_POINT ( 'NONE',  ( 0.05905511811023622659, 1.190944881889763884, -0.8267716535433072833 ) ) ;
#2627 = AXIS2_PLACEMENT_3D ( 'NONE', #10033, #12618, #5235 ) ;
#2628 = ORIENTED_EDGE ( 'NONE', *, *, #1290, .F. ) ;
#2629 = EDGE_CURVE ( 'NONE', #6774, #6775, #842, .T. ) ;
#2630 = ORIENTED_EDGE ( 'NONE', *, *, #5413, .F. ) ;
#2631 = VERTEX_POINT ( 'NONE', #196 ) ;
#2632 = AXIS2_PLACEMENT_3D ( 'NONE', #9090, #3142, #867 ) ;
#2633 = TOROIDAL_SURFACE ( 'NONE', #2888, 0.5590551181102362266, 0.007874015748031495954 ) ;
#2634 = AXIS2_PLACEMENT_3D ( 'NONE', #3594, #14415, #9489 ) ;
#2635 = CARTESIAN_POINT ( 'NONE',  ( 0.3669897256266698715, -0.2952755905511811330, 0.2891647237797818626 ) ) ;
#2636 = CARTESIAN_POINT ( 'NONE',  ( -1.925664620590514131, -2.947732113873157811, 0.02576678317052827349 ) ) ;
#2637 = CIRCLE ( 'NONE', #8644, 0.003937007874015749712 ) ;
#2638 = DIRECTION ( 'NONE',  ( -0.8660254037844347108, 0.000000000000000000, -0.5000000000000069944 ) ) ;
#2639 = FACE_OUTER_BOUND ( 'NONE', #4352, .T. ) ;
#2640 = LINE ( 'NONE', #7550, #14833 ) ;
#2641 = DIRECTION ( 'NONE',  ( -0.4999999999999998335, 0.000000000000000000, -0.8660254037844388186 ) ) ;
#2642 = CARTESIAN_POINT ( 'NONE',  ( -1.882196081866716275, -2.916170042030258092, -0.04518955602145270645 ) ) ;
#2643 = CARTESIAN_POINT ( 'NONE',  ( 0.06278630405416070481, 1.343094588453027427, -0.5877245205702892328 ) ) ;
#2644 = CARTESIAN_POINT ( 'NONE',  ( 0.4854723491485768982, 1.338626482899105241, 0.3484785681409844904 ) ) ;
#2645 = AXIS2_PLACEMENT_3D ( 'NONE', #7414, #1537, #10069 ) ;
#2646 = ORIENTED_EDGE ( 'NONE', *, *, #9551, .F. ) ;
#2647 = ORIENTED_EDGE ( 'NONE', *, *, #3095, .T. ) ;
#2648 = EDGE_CURVE ( 'NONE', #9446, #5934, #3849, .T. ) ;
#2649 = EDGE_LOOP ( 'NONE', ( #8900, #14490, #13904, #14741 ) ) ;
#2650 = CIRCLE ( 'NONE', #4657, 0.04330708661417328326 ) ;
#2651 = ORIENTED_EDGE ( 'NONE', *, *, #5360, .T. ) ;
#2652 = ORIENTED_EDGE ( 'NONE', *, *, #15238, .F. ) ;
#2653 = CARTESIAN_POINT ( 'NONE',  ( -0.4722458785514955237, -0.6629481244416842722, 0.05905511811023622659 ) ) ;
#2654 = EDGE_CURVE ( 'NONE', #10930, #4497, #1592, .T. ) ;
#2655 = AXIS2_PLACEMENT_3D ( 'NONE', #14688, #2762, #1984 ) ;
#2656 = AXIS2_PLACEMENT_3D ( 'NONE', #4257, #12500, #9046 ) ;
#2657 = DIRECTION ( 'NONE',  ( -3.973232667114495301E-16, 0.000000000000000000, 1.000000000000000000 ) ) ;
#2658 = DIRECTION ( 'NONE',  ( -0.000000000000000000, -0.000000000000000000, -1.000000000000000000 ) ) ;
#2659 = DIRECTION ( 'NONE',  ( 0.000000000000000000, 1.000000000000000000, 0.000000000000000000 ) ) ;
#2660 = LINE ( 'NONE', #2567, #12447 ) ;
#2661 = CIRCLE ( 'NONE', #4402, 0.01968503937007874335 ) ;
#2662 = CARTESIAN_POINT ( 'NONE',  ( -1.881874822264153035, -2.917190596920589574, 0.1023714699873570499 ) ) ;
#2663 = ORIENTED_EDGE ( 'NONE', *, *, #13739, .T. ) ;
#2664 = CARTESIAN_POINT ( 'NONE',  ( -1.962487488497034027, -2.889695200659031293, -0.1131027244867615078 ) ) ;
#2665 = CARTESIAN_POINT ( 'NONE',  ( -1.431036756819011213, -0.02829858486107875853, -0.08366141732283460808 ) ) ;
#2666 = DIRECTION ( 'NONE',  ( -0.000000000000000000, -0.000000000000000000, -1.000000000000000000 ) ) ;
#2667 = ORIENTED_EDGE ( 'NONE', *, *, #3280, .T. ) ;
#2668 = VERTEX_POINT ( 'NONE', #1666 ) ;
#2669 = ORIENTED_EDGE ( 'NONE', *, *, #15399, .F. ) ;
#2670 = AXIS2_PLACEMENT_3D ( 'NONE', #3710, #329, #5967 ) ;
#2671 = DIRECTION ( 'NONE',  ( 0.8660254037844347108, 0.000000000000000000, 0.5000000000000069944 ) ) ;
#2672 = EDGE_CURVE ( 'NONE', #8847, #7384, #7339, .T. ) ;
#2673 = TOROIDAL_SURFACE ( 'NONE', #11436, 0.1614173228346456879, 0.003937007874015747977 ) ;
#2674 = CARTESIAN_POINT ( 'NONE',  ( 0.000000000000000000, 0.3543307086614172485, -0.5590551181102362266 ) ) ;
#2675 =( BOUNDED_SURFACE ( )  B_SPLINE_SURFACE ( 3, 2, ( 
 ( #12392, #5084, #1804 ),
 ( #11282, #5308, #6420 ),
 ( #7592, #6562, #1569 ),
 ( #8714, #555, #14579 ),
 ( #4158, #3845, #8629 ),
 ( #6329, #13411, #2680 ),
 ( #7453, #9892, #6254 ),
 ( #11043, #13488, #11128 ),
 ( #5165, #9972, #4009 ),
 ( #8782, #13550, #2815 ) ),
 .UNSPECIFIED., .F., .F., .T. ) 
 B_SPLINE_SURFACE_WITH_KNOTS ( ( 4, 2, 2, 2, 4 ),
 ( 3, 3 ),
 ( 0.004862229905983068978, 0.005359824983622663366, 0.005857420061262256887, 0.006355015138901850408, 0.006852610216541444796 ),
 ( 0.000000000000000000, 1.000000000000000000 ),
 .UNSPECIFIED. ) 
 GEOMETRIC_REPRESENTATION_ITEM ( )  RATIONAL_B_SPLINE_SURFACE ( (
 ( 1.000000000000000000, 0.7071067811865475727, 1.000000000000000000),
 ( 1.000000000000000000, 0.7118664854617688942, 1.000000000000000000),
 ( 1.000000000000000000, 0.7168001159655631449, 1.000000000000000000),
 ( 1.000000000000000000, 0.7268793899691540217, 1.000000000000000000),
 ( 1.000000000000000000, 0.7317766985259492873, 1.000000000000000000),
 ( 1.000000000000000000, 0.7409494124080542310, 1.000000000000000000),
 ( 1.000000000000000000, 0.7450318297967697401, 1.000000000000000000),
 ( 1.000000000000000000, 0.7517743552594693401, 1.000000000000000000),
 ( 1.000000000000000000, 0.7543262850462577607, 1.000000000000000000),
 ( 1.000000000000000000, 0.7558617697692807669, 1.000000000000000000) ) ) 
 REPRESENTATION_ITEM ( '' )  SURFACE ( )  );
#2676 = DIRECTION ( 'NONE',  ( -0.000000000000000000, 0.000000000000000000, 1.000000000000000000 ) ) ;
#2677 = ITEM_DEFINED_TRANSFORMATION ( 'NONE', 'NONE', #4110,  #11481 ) ;
#2679 = AXIS2_PLACEMENT_3D ( 'NONE', #10602, #14287, #14054 ) ;
#2678 = DIRECTION ( 'NONE',  ( -1.000000000000000000, -0.000000000000000000, -0.000000000000000000 ) ) ;
#2680 = CARTESIAN_POINT ( 'NONE',  ( -0.03452177266044149928, -0.1823242888858135624, -0.02287309002717315826 ) ) ;
#2681 = VERTEX_POINT ( 'NONE', #7456 ) ;
#2682 = PLANE ( 'NONE',  #10423 ) ;
#2683 = CARTESIAN_POINT ( 'NONE',  ( 0.2393297813660762718, -0.09842519685039370636, 0.06089400679746260342 ) ) ;
#2684 = VECTOR ( 'NONE', #1954, 39.37007874015748143 ) ;
#2685 = CARTESIAN_POINT ( 'NONE',  ( 0.000000000000000000, -0.4921259842519685179, 0.000000000000000000 ) ) ;
#2686 =( CONVERSION_BASED_UNIT ( 'INCH', #2757 ) LENGTH_UNIT ( ) NAMED_UNIT ( #10348 ) );
#2687 = ORIENTED_EDGE ( 'NONE', *, *, #4030, .T. ) ;
#2688 = ORIENTED_EDGE ( 'NONE', *, *, #11656, .F. ) ;
#2689 = VERTEX_POINT ( 'NONE', #9895 ) ;
#2690 = AXIS2_PLACEMENT_3D ( 'NONE', #10716, #933, #5831 ) ;
#2691 = ORIENTED_EDGE ( 'NONE', *, *, #505, .T. ) ;
#2692 = CARTESIAN_POINT ( 'NONE',  ( 0.09842519685044813504, -0.2952755905511811330, -0.3797276218561366212 ) ) ;
#2693 = CARTESIAN_POINT ( 'NONE',  ( -1.596030944582063960, 0.1136756404979306911, -0.04477369844321314740 ) ) ;
#2694 = AXIS2_PLACEMENT_3D ( 'NONE', #4301, #7600, #7922 ) ;
#2695 = ADVANCED_FACE ( 'NONE', ( #10986 ), #11131, .T. ) ;
#2696 = FACE_OUTER_BOUND ( 'NONE', #8737, .T. ) ;
#2697 = DIRECTION ( 'NONE',  ( 1.000000000000000000, 0.000000000000000000, 0.000000000000000000 ) ) ;
#2698 = DIRECTION ( 'NONE',  ( -1.665334536937734811E-16, 0.5695655044020487834, 0.8219459448134285307 ) ) ;
#2699 = DIRECTION ( 'NONE',  ( 0.8660254037844385966, 0.000000000000000000, -0.4999999999999998890 ) ) ;
#2700 = DIRECTION ( 'NONE',  ( 0.000000000000000000, 0.000000000000000000, -1.000000000000000000 ) ) ;
#2701 = DIRECTION ( 'NONE',  ( 1.224646799147353947E-16, 0.000000000000000000, -1.000000000000000000 ) ) ;
#2702 = EDGE_CURVE ( 'NONE', #6685, #12009, #3781, .T. ) ;
#2703 = CARTESIAN_POINT ( 'NONE',  ( 0.09842519685044814892, -0.2952755905511811330, -0.4190977005962941426 ) ) ;
#2704 = FACE_OUTER_BOUND ( 'NONE', #7858, .T. ) ;
#2705 = AXIS2_PLACEMENT_3D ( 'NONE', #10539, #12018, #9667 ) ;
#2706 = DIRECTION ( 'NONE',  ( 0.8660254037844385966, -0.000000000000000000, 0.5000000000000001110 ) ) ;
#2707 = AXIS2_PLACEMENT_3D ( 'NONE', #9499, #13959, #14105 ) ;
#2708 = ORIENTED_EDGE ( 'NONE', *, *, #5284, .F. ) ;
#2709 = ORIENTED_EDGE ( 'NONE', *, *, #3634, .F. ) ;
#2710 = ORIENTED_EDGE ( 'NONE', *, *, #13432, .T. ) ;
#2711 = EDGE_CURVE ( 'NONE', #6564, #5808, #14860, .T. ) ;
#2712 = CIRCLE ( 'NONE', #1218, 0.03937007874015751446 ) ;
#2713 = EDGE_CURVE ( 'NONE', #12588, #7178, #3574, .T. ) ;
#2714 = CARTESIAN_POINT ( 'NONE',  ( -0.4496668909809726777, -0.2952755905511811330, 0.1459636727603558504 ) ) ;
#2715 = CARTESIAN_POINT ( 'NONE',  ( -1.942693295529114295, -2.938640948109480178, 0.06141235872390152922 ) ) ;
#2716 = LINE ( 'NONE', #14543, #228 ) ;
#2717 = CIRCLE ( 'NONE', #972, 0.1279527559055117780 ) ;
#2718 = PLANE ( 'NONE',  #945 ) ;
#2719 = ADVANCED_FACE ( 'NONE', ( #5240, #10039 ), #8547, .F. ) ;
#2720 = CARTESIAN_POINT ( 'NONE',  ( -1.954276836318071364, -2.867108795541001065, -0.1501860367057778201 ) ) ;
#2721 = LINE ( 'NONE', #9778, #1082 ) ;
#2722 = CARTESIAN_POINT ( 'NONE',  ( 0.000000000000000000, 0.1692468441617604180, -0.03937007874015747977 ) ) ;
#2723 = CARTESIAN_POINT ( 'NONE',  ( -1.880688305523271708, -2.919848346818194162, -0.02845389545398609513 ) ) ;
#2724 = CARTESIAN_POINT ( 'NONE',  ( 0.05905511811023621271, 1.338877467290996659, -0.5922895726594219479 ) ) ;
#2725 = CYLINDRICAL_SURFACE ( 'NONE', #407, 0.03937007874015761161 ) ;
#2726 = ORIENTED_EDGE ( 'NONE', *, *, #14605, .F. ) ;
#2727 = ORIENTED_EDGE ( 'NONE', *, *, #5996, .F. ) ;
#2728 = VERTEX_POINT ( 'NONE', #13414 ) ;
#2729 = ORIENTED_EDGE ( 'NONE', *, *, #3949, .T. ) ;
#2730 = EDGE_LOOP ( 'NONE', ( #12534, #3767, #11892, #9821 ) ) ;
#2731 = EDGE_CURVE ( 'NONE', #3678, #9959, #7371, .T. ) ;
#2732 = CARTESIAN_POINT ( 'NONE',  ( -0.5084014747882513729, -0.4881889763779528324, 0.2935257283253980831 ) ) ;
#2733 = DIRECTION ( 'NONE',  ( 0.000000000000000000, 0.000000000000000000, 1.000000000000000000 ) ) ;
#2734 = CARTESIAN_POINT ( 'NONE',  ( 0.000000000000000000, -0.4921259842519685179, 0.1574803149606299191 ) ) ;
#2735 = EDGE_CURVE ( 'NONE', #14790, #14788, #7584, .T. ) ;
#2736 = CARTESIAN_POINT ( 'NONE',  ( -0.5412478373021294420, 1.035433070866141891, 0.2362233606508100381 ) ) ;
#2737 = DIRECTION ( 'NONE',  ( 0.000000000000000000, 0.000000000000000000, 1.000000000000000000 ) ) ;
#2738 = CARTESIAN_POINT ( 'NONE',  ( 0.05905511811023622659, 1.043263280880422528, -0.5946706712680680518 ) ) ;
#2739 = CARTESIAN_POINT ( 'NONE',  ( -1.900558757413772559, -2.942139299165188238, -0.05093160179085944039 ) ) ;
#2740 = VERTEX_POINT ( 'NONE', #4162 ) ;
#2741 = DIRECTION ( 'NONE',  ( 0.5000000000000001110, 0.000000000000000000, -0.8660254037844385966 ) ) ;
#2742 = CARTESIAN_POINT ( 'NONE',  ( -1.568343923620152625, 0.1178486908565804098, 0.05905511811023622659 ) ) ;
#2743 = CARTESIAN_POINT ( 'NONE',  ( -1.409031571664937754, -0.006876126661574346287, -0.06053688359312208583 ) ) ;
#2744 = ORIENTED_EDGE ( 'NONE', *, *, #11806, .F. ) ;
#2745 = EDGE_CURVE ( 'NONE', #15416, #4326, #10336, .T. ) ;
#2746 = VERTEX_POINT ( 'NONE', #13795 ) ;
#2747 = VERTEX_POINT ( 'NONE', #3060 ) ;
#2748 = CARTESIAN_POINT ( 'NONE',  ( 0.1017691531708310448, -0.2952755905511811330, 0.7406662147377752747 ) ) ;
#2749 = DIRECTION ( 'NONE',  ( 1.000000000000000000, 0.000000000000000000, 0.000000000000000000 ) ) ;
#2750 = DIRECTION ( 'NONE',  ( 0.000000000000000000, 0.000000000000000000, 1.000000000000000000 ) ) ;
#2751 = DIRECTION ( 'NONE',  ( -0.000000000000000000, -0.000000000000000000, 1.000000000000000000 ) ) ;
#2752 = ORIENTED_EDGE ( 'NONE', *, *, #14129, .T. ) ;
#2753 = CARTESIAN_POINT ( 'NONE',  ( 1.976792077363838002E-17, 5.629100846319917971E-17, 0.1614173228346456879 ) ) ;
#2754 = DIRECTION ( 'NONE',  ( -0.000000000000000000, -0.000000000000000000, -1.000000000000000000 ) ) ;
#2755 = CARTESIAN_POINT ( 'NONE',  ( -0.06327586242532841354, -0.1861954285973654311, 0.03830155300069465474 ) ) ;
#2756 = EDGE_CURVE ( 'NONE', #3058, #9379, #2336, .T. ) ;
#2757 = LENGTH_MEASURE_WITH_UNIT ( LENGTH_MEASURE( 0.02539999999999999897 ), #7375 );
#2758 = ADVANCED_BREP_SHAPE_REPRESENTATION ( '', ( #9613, #14728, #11481 ), #14478 ) ;
#2759 = ORIENTED_EDGE ( 'NONE', *, *, #13524, .F. ) ;
#2760 = VERTEX_POINT ( 'NONE', #11454 ) ;
#2761 = EDGE_LOOP ( 'NONE', ( #3278, #5053, #7756, #12785 ) ) ;
#2762 = DIRECTION ( 'NONE',  ( -0.000000000000000000, 0.000000000000000000, 1.000000000000000000 ) ) ;
#2763 = CARTESIAN_POINT ( 'NONE',  ( 0.000000000000000000, 2.637795275590551825, -0.03937007874015747977 ) ) ;
#2764 = CARTESIAN_POINT ( 'NONE',  ( 1.181102362204724310, 4.044111181948214319E-16, -0.02952755905511811330 ) ) ;
#2765 = SHAPE_DEFINITION_REPRESENTATION ( #7419, #8904 ) ;
#2766 = CARTESIAN_POINT ( 'NONE',  ( -1.411112778431387937, -0.007856062364883056523, 0.06231671783893451277 ) ) ;
#2767 = CARTESIAN_POINT ( 'NONE',  ( 0.000000000000000000, 1.614173228346457156, 0.000000000000000000 ) ) ;
#2768 = CARTESIAN_POINT ( 'NONE',  ( 7.232166136696967594E-17, 0.3070866141732283561, 0.5905511811023621549 ) ) ;
#2769 = CARTESIAN_POINT ( 'NONE',  ( 0.1181102362204723977, 2.444206406002937815, 0.03937007874015747977 ) ) ;
#2770 = ORIENTED_EDGE ( 'NONE', *, *, #14019, .T. ) ;
#2771 = ORIENTED_EDGE ( 'NONE', *, *, #2313, .T. ) ;
#2772 = EDGE_LOOP ( 'NONE', ( #14701, #14993 ) ) ;
#2773 = ORIENTED_EDGE ( 'NONE', *, *, #3664, .T. ) ;
#2774 = EDGE_CURVE ( 'NONE', #11438, #6858, #15369, .T. ) ;
#2775 = DIRECTION ( 'NONE',  ( -0.8660254037844398178, 0.000000000000000000, 0.4999999999999979461 ) ) ;
#2776 = CARTESIAN_POINT ( 'NONE',  ( -1.953726846202070933, -2.911621419847214121, 0.08674134307398276289 ) ) ;
#2777 =( NAMED_UNIT ( * ) SI_UNIT ( $, .STERADIAN. ) SOLID_ANGLE_UNIT ( ) );
#2778 = DIRECTION ( 'NONE',  ( -0.8221763679505030842, 0.000000000000000000, -0.5692328345973368675 ) ) ;
#2779 = DIRECTION ( 'NONE',  ( -4.292327424963298981E-16, 1.000000000000000000, 2.478176394252600369E-16 ) ) ;
#2780 = DIRECTION ( 'NONE',  ( -0.000000000000000000, -1.000000000000000000, -0.000000000000000000 ) ) ;
#2781 = CARTESIAN_POINT ( 'NONE',  ( -1.930585417187773434, -2.789123413658596284, -0.1561196149103405983 ) ) ;
#2782 = EDGE_CURVE ( 'NONE', #5753, #3506, #4392, .T. ) ;
#2783 = DIRECTION ( 'NONE',  ( -1.000000000000000000, 0.000000000000000000, 0.000000000000000000 ) ) ;
#2784 = LINE ( 'NONE', #10947, #1655 ) ;
#2785 = ADVANCED_FACE ( 'NONE', ( #6803, #7759 ), #558, .F. ) ;
#2786 = ORIENTED_EDGE ( 'NONE', *, *, #13481, .F. ) ;
#2787 = EDGE_LOOP ( 'NONE', ( #9470, #11496, #5471, #4708 ) ) ;
#2788 = ORIENTED_EDGE ( 'NONE', *, *, #3042, .T. ) ;
#2789 = ORIENTED_EDGE ( 'NONE', *, *, #8631, .F. ) ;
#2790 = ADVANCED_FACE ( 'NONE', ( #7996 ), #1349, .F. ) ;
#2791 = ORIENTED_EDGE ( 'NONE', *, *, #13314, .F. ) ;
#2792 = DIRECTION ( 'NONE',  ( 0.000000000000000000, 0.000000000000000000, -1.000000000000000000 ) ) ;
#2793 = CARTESIAN_POINT ( 'NONE',  ( 0.000000000000000000, 0.07874015748031495954, -0.05298991407461853265 ) ) ;
#2794 = PRODUCT_DEFINITION_SHAPE ( 'NONE', 'NONE',  #15490 ) ;
#2795 = DIRECTION ( 'NONE',  ( 0.000000000000000000, 0.000000000000000000, 1.000000000000000000 ) ) ;
#2796 = CARTESIAN_POINT ( 'NONE',  ( 0.09061599198715353243, 0.000000000000000000, 0.007444810018878659542 ) ) ;
#2797 = CARTESIAN_POINT ( 'NONE',  ( 0.7205731843802273273, 1.190944881889763884, 0.4842140986486808130 ) ) ;
#2798 = CARTESIAN_POINT ( 'NONE',  ( 0.000000000000000000, 0.4133858267716535306, -0.03937007874015747977 ) ) ;
#2799 = CARTESIAN_POINT ( 'NONE',  ( -1.898411911810662378, -2.948034399344904521, 0.02614368185018839039 ) ) ;
#2800 = EDGE_LOOP ( 'NONE', ( #9739, #7019, #10849 ) ) ;
#2801 = CYLINDRICAL_SURFACE ( 'NONE', #11695, 0.5511811023622046335 ) ;
#2802 = EDGE_CURVE ( 'NONE', #11638, #14035, #5331, .T. ) ;
#2803 = CARTESIAN_POINT ( 'NONE',  ( -1.586197524891038269, 0.1268408028903934559, 0.05897664633264051298 ) ) ;
#2804 = DIRECTION ( 'NONE',  ( 0.000000000000000000, 0.000000000000000000, 1.000000000000000000 ) ) ;
#2805 = EDGE_CURVE ( 'NONE', #8036, #7766, #9255, .T. ) ;
#2806 = ORIENTED_EDGE ( 'NONE', *, *, #6170, .T. ) ;
#2807 = ORIENTED_EDGE ( 'NONE', *, *, #11515, .T. ) ;
#2808 = ADVANCED_FACE ( 'NONE', ( #15049 ), #13099, .T. ) ;
#2809 = EDGE_CURVE ( 'NONE', #12857, #5735, #5399, .T. ) ;
#2810 = ORIENTED_EDGE ( 'NONE', *, *, #7321, .F. ) ;
#2811 = DIRECTION ( 'NONE',  ( 1.000000000000000000, 0.000000000000000000, 0.000000000000000000 ) ) ;
#2812 = FACE_OUTER_BOUND ( 'NONE', #6071, .T. ) ;
#2813 = DIRECTION ( 'NONE',  ( 1.000000000000000000, -0.000000000000000000, -0.000000000000000000 ) ) ;
#2814 = CARTESIAN_POINT ( 'NONE',  ( 0.1181102362204724254, 2.448818897637795367, -0.03937007874015747977 ) ) ;
#2815 = CARTESIAN_POINT ( 'NONE',  ( -0.01854992166427318900, -0.1800031784444983685, 0.005378007177148339153 ) ) ;
#2816 = ORIENTED_EDGE ( 'NONE', *, *, #2227, .F. ) ;
#2817 = DIRECTION ( 'NONE',  ( 0.000000000000000000, 0.000000000000000000, -1.000000000000000000 ) ) ;
#2818 = CARTESIAN_POINT ( 'NONE',  ( 0.000000000000000000, 0.3622047244094487306, 0.000000000000000000 ) ) ;
#2819 = AXIS2_PLACEMENT_3D ( 'NONE', #12725, #12788, #2045 ) ;
#2820 = CIRCLE ( 'NONE', #11319, 0.003937007874015721089 ) ;
#2821 = CARTESIAN_POINT ( 'NONE',  ( -0.002197004598026061628, -0.1775723205537574900, -0.001204381035045432730 ) ) ;
#2822 = VECTOR ( 'NONE', #5047, 39.37007874015748143 ) ;
#2823 = CARTESIAN_POINT ( 'NONE',  ( -0.2652685895081163259, -0.4921259842519685179, 0.03495519865516327068 ) ) ;
#2824 = AXIS2_PLACEMENT_3D ( 'NONE', #5816, #10618, #51 ) ;
#2825 = EDGE_LOOP ( 'NONE', ( #14455, #6216, #8777 ) ) ;
#2826 = ADVANCED_FACE ( 'NONE', ( #7690 ), #1836, .T. ) ;
#2827 = ORIENTED_EDGE ( 'NONE', *, *, #8540, .F. ) ;
#2828 = ORIENTED_EDGE ( 'NONE', *, *, #36, .T. ) ;
#2829 = CARTESIAN_POINT ( 'NONE',  ( 0.000000000000000000, 1.425196850393700920, 0.000000000000000000 ) ) ;
#2830 = DIRECTION ( 'NONE',  ( -0.08093398607328358696, -0.9967194639908912857, 1.383226122518415193E-14 ) ) ;
#2831 = AXIS2_PLACEMENT_3D ( 'NONE', #9774, #6219, #10938 ) ;
#2832 = AXIS2_PLACEMENT_3D ( 'NONE', #12746, #10068, #462 ) ;
#2833 = ADVANCED_FACE ( 'NONE', ( #5483 ), #12478, .T. ) ;
#2834 = VECTOR ( 'NONE', #5316, 39.37007874015748854 ) ;
#2835 = EDGE_CURVE ( 'NONE', #11283, #6857, #12601, .T. ) ;
#2836 = FACE_OUTER_BOUND ( 'NONE', #8922, .T. ) ;
#2837 = CARTESIAN_POINT ( 'NONE',  ( 0.05905511811023622659, 1.190944881889763884, -0.8267716535433072833 ) ) ;
#2838 = AXIS2_PLACEMENT_3D ( 'NONE', #1438, #3934, #417 ) ;
#2839 = DIRECTION ( 'NONE',  ( 1.942890293094023946E-16, 0.9706086590632821975, 0.2406633145109098315 ) ) ;
#2840 = LINE ( 'NONE', #435, #6092 ) ;
#2841 = CARTESIAN_POINT ( 'NONE',  ( -1.181102362204724310, -0.1279527559055117225, 0.02952755905511811330 ) ) ;
#2842 = DIRECTION ( 'NONE',  ( -1.000000000000000000, -0.000000000000000000, -0.000000000000000000 ) ) ;
#2843 = CARTESIAN_POINT ( 'NONE',  ( 0.1552072824047652233, -0.003937007874015747977, -0.5870514566507987197 ) ) ;
#2844 = CIRCLE ( 'NONE', #1857, 0.003937007874015747977 ) ;
#2845 = AXIS2_PLACEMENT_3D ( 'NONE', #1292, #7241, #1451 ) ;
#2846 = ORIENTED_EDGE ( 'NONE', *, *, #9322, .T. ) ;
#2847 = AXIS2_PLACEMENT_3D ( 'NONE', #1521, #14606, #1454 ) ;
#2848 = DIRECTION ( 'NONE',  ( 1.000000000000000000, 0.000000000000000000, 0.000000000000000000 ) ) ;
#2849 = AXIS2_PLACEMENT_3D ( 'NONE', #14886, #13713, #13940 ) ;
#2850 = ORIENTED_EDGE ( 'NONE', *, *, #1570, .T. ) ;
#2851 = TOROIDAL_SURFACE ( 'NONE', #2351, 0.007874015748031495954, 0.003937007874015747977 ) ;
#2852 = EDGE_LOOP ( 'NONE', ( #7750, #8181, #91, #8167 ) ) ;
#2853 = AXIS2_PLACEMENT_3D ( 'NONE', #7619, #5421, #11147 ) ;
#2854 = DIRECTION ( 'NONE',  ( 0.000000000000000000, 0.000000000000000000, 1.000000000000000000 ) ) ;
#2855 = CARTESIAN_POINT ( 'NONE',  ( -1.948408827770508722, -2.924691321014698531, -0.06190742950379295867 ) ) ;
#2856 = AXIS2_PLACEMENT_3D ( 'NONE', #9512, #13321, #2588 ) ;
#2857 = TOROIDAL_SURFACE ( 'NONE', #1614, 0.5433070866141731514, 0.007874015748031495954 ) ;
#2858 = AXIS2_PLACEMENT_3D ( 'NONE', #7016, #9290, #14066 ) ;
#2859 = CLOSED_SHELL ( 'NONE', ( #5798, #3468, #6553, #7889, #1207, #4927, #5474, #1562, #822, #6358, #1578, #8350, #10726, #7898, #7963, #11257, #15332 ) ) ;
#2860 = AXIS2_PLACEMENT_3D ( 'NONE', #13789, #12841, #8056 ) ;
#2861 = DIRECTION ( 'NONE',  ( 1.000000000000000000, 0.000000000000000000, 0.000000000000000000 ) ) ;
#2862 = DIRECTION ( 'NONE',  ( 0.000000000000000000, 0.000000000000000000, 1.000000000000000000 ) ) ;
#2863 = CIRCLE ( 'NONE', #7616, 0.003937007874015741038 ) ;
#2864 = CARTESIAN_POINT ( 'NONE',  ( 0.000000000000000000, -1.707404996040164512E-17, 0.000000000000000000 ) ) ;
#2865 = CARTESIAN_POINT ( 'NONE',  ( -1.887612226072282740, -2.902832404796057197, 0.07695804445277183714 ) ) ;
#2866 = DIRECTION ( 'NONE',  ( -1.000000000000000000, 0.000000000000000000, 0.000000000000000000 ) ) ;
#2867 = CYLINDRICAL_SURFACE ( 'NONE', #10164, 0.01968503937007875723 ) ;
#2868 = VERTEX_POINT ( 'NONE', #7920 ) ;
#2869 = EDGE_LOOP ( 'NONE', ( #6859, #236, #15192, #15371 ) ) ;
#2870 = CIRCLE ( 'NONE', #14148, 0.003937007874015758385 ) ;
#2871 = ORIENTED_EDGE ( 'NONE', *, *, #11557, .F. ) ;
#2872 = CIRCLE ( 'NONE', #11642, 0.003937007874015724558 ) ;
#2873 = AXIS2_PLACEMENT_3D ( 'NONE', #13466, #8689, #1636 ) ;
#2874 = EDGE_LOOP ( 'NONE', ( #10650, #237, #8309, #5642 ) ) ;
#2875 = ORIENTED_EDGE ( 'NONE', *, *, #6322, .T. ) ;
#2876 = AXIS2_PLACEMENT_3D ( 'NONE', #8695, #13469, #3757 ) ;
#2877 = CARTESIAN_POINT ( 'NONE',  ( -1.397634627758906012, -0.02569727825916744493, -0.06948688383644625877 ) ) ;
#2878 = EDGE_CURVE ( 'NONE', #3695, #14360, #2350, .T. ) ;
#2879 = CARTESIAN_POINT ( 'NONE',  ( -0.5860051159906336515, -0.09842519685039370636, 0.1591122789105256785 ) ) ;
#2880 = CARTESIAN_POINT ( 'NONE',  ( 0.000000000000000000, 0.4094488188976377896, 0.000000000000000000 ) ) ;
#2881 = ADVANCED_FACE ( 'NONE', ( #6498 ), #11285, .F. ) ;
#2882 = CARTESIAN_POINT ( 'NONE',  ( -2.169366242005649870, -2.077173998931367560, 0.09331536252806132969 ) ) ;
#2883 = DIRECTION ( 'NONE',  ( 0.8660254037844405950, 2.369676336725575161E-14, -0.4999999999999967804 ) ) ;
#2884 = DIRECTION ( 'NONE',  ( 0.000000000000000000, 0.000000000000000000, -1.000000000000000000 ) ) ;
#2885 = LINE ( 'NONE', #8837, #7568 ) ;
#2886 = AXIS2_PLACEMENT_3D ( 'NONE', #5358, #10389, #4203 ) ;
#2887 = DIRECTION ( 'NONE',  ( -0.000000000000000000, -1.000000000000000000, -0.000000000000000000 ) ) ;
#2888 = AXIS2_PLACEMENT_3D ( 'NONE', #2521, #6113, #7296 ) ;
#2889 = CARTESIAN_POINT ( 'NONE',  ( -1.884711123585276482, -2.909996678602419173, -0.06153400971538078301 ) ) ;
#2890 = AXIS2_PLACEMENT_3D ( 'NONE', #2135, #2216, #8174 ) ;
#2891 = ORIENTED_EDGE ( 'NONE', *, *, #4816, .F. ) ;
#2892 = CARTESIAN_POINT ( 'NONE',  ( -2.011807227224585048, -2.756102811318752011, -0.1765457041329582810 ) ) ;
#2893 = B_SPLINE_CURVE_WITH_KNOTS ( 'NONE', 3,
 ( #13760, #3023, #5513, #3974, #13516, #11169 ),
 .UNSPECIFIED., .F., .F.,
 ( 4, 2, 4 ),
 ( -1.812139438552513428E-05, 0.0003725414720542789089, 0.0007632043384940828809 ),
 .UNSPECIFIED. ) ;
#2894 = ADVANCED_FACE ( 'NONE', ( #10574 ), #5866, .T. ) ;
#2895 = DIRECTION ( 'NONE',  ( -0.000000000000000000, -1.000000000000000000, -0.000000000000000000 ) ) ;
#2896 = AXIS2_PLACEMENT_3D ( 'NONE', #2391, #8029, #8204 ) ;
#2897 = CARTESIAN_POINT ( 'NONE',  ( 0.000000000000000000, 2.637795275590551825, 0.03937007874015747977 ) ) ;
#2898 = VERTEX_POINT ( 'NONE', #10504 ) ;
#2899 = EDGE_LOOP ( 'NONE', ( #2580, #2204, #14160, #2173 ) ) ;
#2901 = VERTEX_POINT ( 'NONE', #12847 ) ;
#2900 = TOROIDAL_SURFACE ( 'NONE', #11400, 1.885039370078740451, 0.01968503937007873988 ) ;
#2902 = AXIS2_PLACEMENT_3D ( 'NONE', #9374, #5989, #920 ) ;
#2903 = CIRCLE ( 'NONE', #3662, 0.2106299212598415904 ) ;
#2904 = EDGE_CURVE ( 'NONE', #1832, #10243, #2206, .T. ) ;
#2905 = TOROIDAL_SURFACE ( 'NONE', #2418, 0.04330708661417328326, 0.003937007874015747977 ) ;
#2906 = EDGE_CURVE ( 'NONE', #6855, #5486, #7461, .T. ) ;
#2907 = DIRECTION ( 'NONE',  ( 1.000000000000000000, 0.000000000000000000, 0.000000000000000000 ) ) ;
#2908 = DIRECTION ( 'NONE',  ( 0.000000000000000000, -1.000000000000000000, 0.000000000000000000 ) ) ;
#2909 = DIRECTION ( 'NONE',  ( 0.000000000000000000, 0.000000000000000000, 1.000000000000000000 ) ) ;
#2910 = DIRECTION ( 'NONE',  ( 0.03006568382583901106, 0.9995479251422039191, 0.000000000000000000 ) ) ;
#2911 = DIRECTION ( 'NONE',  ( 0.7666137478421605200, -0.6421085279136201640, 0.000000000000000000 ) ) ;
#2912 = ORIENTED_EDGE ( 'NONE', *, *, #10564, .F. ) ;
#2913 = CYLINDRICAL_SURFACE ( 'NONE', #11163, 0.003937007874015721089 ) ;
#2914 = ADVANCED_FACE ( 'NONE', ( #2273 ), #6853, .T. ) ;
#2915 = CARTESIAN_POINT ( 'NONE',  ( -0.4857119623810620679, 1.338597318737259734, 0.3486169089052708614 ) ) ;
#2916 = DIRECTION ( 'NONE',  ( -0.000000000000000000, -1.000000000000000000, -0.000000000000000000 ) ) ;
#2917 = CIRCLE ( 'NONE', #7405, 0.003937007874015758385 ) ;
#2918 = DIRECTION ( 'NONE',  ( 0.000000000000000000, 0.000000000000000000, -1.000000000000000000 ) ) ;
#2919 = SPHERICAL_SURFACE ( 'NONE', #12347, 0.003937007874015747977 ) ;
#2920 =( LENGTH_UNIT ( ) NAMED_UNIT ( * ) SI_UNIT ( $, .METRE. ) );
#2921 = AXIS2_PLACEMENT_3D ( 'NONE', #4472, #9253, #3293 ) ;
#2922 = EDGE_LOOP ( 'NONE', ( #3582, #12448, #11039, #6838 ) ) ;
#2923 = CIRCLE ( 'NONE', #8187, 0.003937007874015749712 ) ;
#2924 = ORIENTED_EDGE ( 'NONE', *, *, #5467, .F. ) ;
#2925 = EDGE_LOOP ( 'NONE', ( #3616, #13200, #7237, #10231 ) ) ;
#2926 = CARTESIAN_POINT ( 'NONE',  ( 0.5452492930724234244, 1.043307086614173373, 0.2466088494548703824 ) ) ;
#2927 = DIRECTION ( 'NONE',  ( 0.000000000000000000, -1.000000000000000000, -0.000000000000000000 ) ) ;
#2928=STYLED_ITEM('',(#15519),#9754);
#2929 = ADVANCED_FACE ( 'NONE', ( #960 ), #2119, .T. ) ;
#2930 = CARTESIAN_POINT ( 'NONE',  ( -2.111939568874931616, -2.009758264533141769, 0.1096046912080334140 ) ) ;
#2931 = CARTESIAN_POINT ( 'NONE',  ( -0.5418660417173573052, -0.4921259842519685179, 0.2355633981508970520 ) ) ;
#2932 = DIRECTION ( 'NONE',  ( -0.2084205441254165792, 0.9706086590632808653, -0.1203316572554584685 ) ) ;
#2933 = DIRECTION ( 'NONE',  ( 0.000000000000000000, -1.000000000000000000, -0.000000000000000000 ) ) ;
#2934 = CIRCLE ( 'NONE', #6931, 0.003937007874015758385 ) ;
#2935 = LINE ( 'NONE', #5255, #380 ) ;
#2936 = DIRECTION ( 'NONE',  ( -0.8660254037844427044, 0.000000000000000000, 0.4999999999999929501 ) ) ;
#2937 = EDGE_CURVE ( 'NONE', #6855, #13421, #6980, .T. ) ;
#2938 = DIRECTION ( 'NONE',  ( 1.000000000000000000, 0.000000000000000000, 3.476578583725179813E-16 ) ) ;
#2939 = VECTOR ( 'NONE', #1027, 39.37007874015748143 ) ;
#2940 = FACE_BOUND ( 'NONE', #7783, .T. ) ;
#2941 = CARTESIAN_POINT ( 'NONE',  ( 0.000000000000000000, 2.393700787401575436, 0.000000000000000000 ) ) ;
#2942 = CIRCLE ( 'NONE', #11440, 0.01968503937007872948 ) ;
#2943 = EDGE_LOOP ( 'NONE', ( #15010, #14056, #14070, #2786 ) ) ;
#2944 = ADVANCED_FACE ( 'NONE', ( #7215 ), #13860, .T. ) ;
#2945 = FACE_OUTER_BOUND ( 'NONE', #8530, .T. ) ;
#2946 = ORIENTED_EDGE ( 'NONE', *, *, #1468, .F. ) ;
#2947=STYLED_ITEM('',(#15533),#14728);
#2948 = ORIENTED_EDGE ( 'NONE', *, *, #7727, .T. ) ;
#2949 = FACE_OUTER_BOUND ( 'NONE', #7696, .T. ) ;
#2950 = CARTESIAN_POINT ( 'NONE',  ( -0.1023622047242991467, -0.2952755905511811330, -0.4624047872104675161 ) ) ;
#2951 = TOROIDAL_SURFACE ( 'NONE', #3457, 0.04330708661417326938, 0.003937007874015747977 ) ;
#2952 = DIRECTION ( 'NONE',  ( 0.000000000000000000, -1.000000000000000000, 0.000000000000000000 ) ) ;
#2953 = DIRECTION ( 'NONE',  ( 0.000000000000000000, 1.000000000000000000, 0.000000000000000000 ) ) ;
#2954 = CIRCLE ( 'NONE', #12224, 0.03937007874015751446 ) ;
#2955 = SPHERICAL_SURFACE ( 'NONE', #2886, 0.003937007874015747977 ) ;
#2956 = CARTESIAN_POINT ( 'NONE',  ( -1.941802290328372038, -2.756726374736679031, 0.1575978286346828017 ) ) ;
#2957 = CARTESIAN_POINT ( 'NONE',  ( 0.5398975377803496567, -0.4921259842519685179, 0.2389729469846946508 ) ) ;
#2958 = FACE_OUTER_BOUND ( 'NONE', #338, .T. ) ;
#2959 = ORIENTED_EDGE ( 'NONE', *, *, #13432, .F. ) ;
#2960 = EDGE_CURVE ( 'NONE', #14556, #7004, #8117, .T. ) ;
#2961 = ORIENTED_EDGE ( 'NONE', *, *, #4679, .T. ) ;
#2962 = AXIS2_PLACEMENT_3D ( 'NONE', #13728, #7754, #10113 ) ;
#2963 = VERTEX_POINT ( 'NONE', #19 ) ;
#2964 = ORIENTED_EDGE ( 'NONE', *, *, #2355, .T. ) ;
#2965 = ORIENTED_EDGE ( 'NONE', *, *, #1680, .T. ) ;
#2966 = CIRCLE ( 'NONE', #6706, 0.003937007874015724558 ) ;
#2967 = CARTESIAN_POINT ( 'NONE',  ( -1.411805157433859925, -0.008165521224367720821, -0.06278203852593729206 ) ) ;
#2968 = CARTESIAN_POINT ( 'NONE',  ( 0.9851651268172137987, -1.725292181286280480, 0.08366141732283420562 ) ) ;
#2969 = CARTESIAN_POINT ( 'NONE',  ( 0.000000000000000000, 0.003937007874015860734, 0.000000000000000000 ) ) ;
#2970 = DIRECTION ( 'NONE',  ( 0.000000000000000000, 0.000000000000000000, 1.000000000000000000 ) ) ;
#2971 = CARTESIAN_POINT ( 'NONE',  ( 0.5615510810874363434, -0.1023622047244094474, 0.2014679098129276424 ) ) ;
#2972 = CARTESIAN_POINT ( 'NONE',  ( 6.653592845761209348E-17, 2.393700787401575436, -0.5433070866141731514 ) ) ;
#2973 = DIRECTION ( 'NONE',  ( -0.000000000000000000, -1.000000000000000000, -0.000000000000000000 ) ) ;
#2974 = DIRECTION ( 'NONE',  ( -1.000000000000000000, -0.000000000000000000, -0.000000000000000000 ) ) ;
#2975 = CARTESIAN_POINT ( 'NONE',  ( -1.880311997174697103, -2.920764059707957383, -0.02288515043993272213 ) ) ;
#2976 = EDGE_LOOP ( 'NONE', ( #9926, #13230, #2009, #829 ) ) ;
#2977 = CARTESIAN_POINT ( 'NONE',  ( -2.182693454834259139, -1.630005269948474167, -0.1033464566929131884 ) ) ;
#2978 = CARTESIAN_POINT ( 'NONE',  ( -0.5452492930724200937, 1.338582677165354395, 0.2466088494548780152 ) ) ;
#2979 = VERTEX_POINT ( 'NONE', #4779 ) ;
#2980 = ORIENTED_EDGE ( 'NONE', *, *, #3489, .F. ) ;
#2981 = UNCERTAINTY_MEASURE_WITH_UNIT (LENGTH_MEASURE( 1.000000000000000082E-05 ), #15165, 'distance_accuracy_value', 'NONE');
#2982 = ORIENTED_EDGE ( 'NONE', *, *, #11548, .T. ) ;
#2983 = CARTESIAN_POINT ( 'NONE',  ( 0.05905511811023622659, 1.043307086614173373, -0.5946706712680680518 ) ) ;
#2984 = ADVANCED_FACE ( 'NONE', ( #9564 ), #12360, .T. ) ;
#2985 = CARTESIAN_POINT ( 'NONE',  ( -0.4330708661417336236, -0.003937007874015747977, 0.4318761856142863120 ) ) ;
#2986 = FACE_OUTER_BOUND ( 'NONE', #2101, .T. ) ;
#2987 = CARTESIAN_POINT ( 'NONE',  ( 0.2642136714278430776, -0.4881889763779528324, 0.03889220652927401906 ) ) ;
#2988 = CARTESIAN_POINT ( 'NONE',  ( -0.3964138223131424832, -0.2952755905511811330, 0.1515865201236451798 ) ) ;
#2989 = FACE_OUTER_BOUND ( 'NONE', #14058, .T. ) ;
#2990 = EDGE_LOOP ( 'NONE', ( #967, #4378, #8963 ) ) ;
#2991 = DIRECTION ( 'NONE',  ( 0.5000000000000001110, -0.000000000000000000, -0.8660254037844388186 ) ) ;
#2992 = DIRECTION ( 'NONE',  ( 1.445602896647339903E-16, 0.000000000000000000, -1.000000000000000000 ) ) ;
#2993 = DIRECTION ( 'NONE',  ( 1.000000000000000000, -8.673617379884087537E-15, 1.504632769052536530E-28 ) ) ;
#2994 = CARTESIAN_POINT ( 'NONE',  ( -1.224409448818897461, 5.303588500244450842E-18, 0.02559055118110236185 ) ) ;
#2995 = FACE_OUTER_BOUND ( 'NONE', #2063, .T. ) ;
#2996 = EDGE_CURVE ( 'NONE', #10010, #3213, #1262, .T. ) ;
#2997 = ADVANCED_FACE ( 'NONE', ( #3607 ), #5593, .T. ) ;
#2998 = ORIENTED_EDGE ( 'NONE', *, *, #14986, .F. ) ;
#2999 = VERTEX_POINT ( 'NONE', #4847 ) ;
#3000 =( REPRESENTATION_RELATIONSHIP ('NONE','NONE', #8904, #2403 ) REPRESENTATION_RELATIONSHIP_WITH_TRANSFORMATION ( #4486 )SHAPE_REPRESENTATION_RELATIONSHIP( ) );
#3001 = EDGE_CURVE ( 'NONE', #13986, #7182, #8239, .T. ) ;
#3002 = DIRECTION ( 'NONE',  ( -0.000000000000000000, 1.000000000000000000, -0.000000000000000000 ) ) ;
#3003 = CARTESIAN_POINT ( 'NONE',  ( -0.07278938515219078587, 0.1649651754371201928, -0.05936614484719852924 ) ) ;
#3004 = CARTESIAN_POINT ( 'NONE',  ( 0.2681506793018588186, -0.1023622047244094474, 0.03207310886168000114 ) ) ;
#3005 = SHAPE_DEFINITION_REPRESENTATION ( #13914, #11075 ) ;
#3006 = DIRECTION ( 'NONE',  ( 0.000000000000000000, 0.000000000000000000, -1.000000000000000000 ) ) ;
#3007 = DIRECTION ( 'NONE',  ( 0.000000000000000000, 0.000000000000000000, -1.000000000000000000 ) ) ;
#3008 = CARTESIAN_POINT ( 'NONE',  ( -2.184126211765463843, -1.902526540362033503, -0.08609155816397313921 ) ) ;
#3009 = CARTESIAN_POINT ( 'NONE',  ( 0.1618514667033794374, -0.4881889763779528324, 0.2161887458866224576 ) ) ;
#3010 = CARTESIAN_POINT ( 'NONE',  ( -2.464375602680784816, 0.7077922088437123005, 0.1033464566929134798 ) ) ;
#3011 = EDGE_CURVE ( 'NONE', #2963, #3832, #5711, .T. ) ;
#3012 = CARTESIAN_POINT ( 'NONE',  ( 0.4854723491485768982, 1.338626482899105241, 0.3484785681409844904 ) ) ;
#3013 = ORIENTED_EDGE ( 'NONE', *, *, #7286, .T. ) ;
#3014 = ADVANCED_FACE ( 'NONE', ( #3532 ), #3294, .F. ) ;
#3015 = ORIENTED_EDGE ( 'NONE', *, *, #8331, .T. ) ;
#3016 = LINE ( 'NONE', #11721, #11627 ) ;
#3017 = ORIENTED_EDGE ( 'NONE', *, *, #3386, .F. ) ;
#3018 = EDGE_LOOP ( 'NONE', ( #9771, #12351, #5309, #9353 ) ) ;
#3019 = EDGE_CURVE ( 'NONE', #12501, #2740, #9621, .T. ) ;
#3020 = ADVANCED_FACE ( 'NONE', ( #7575 ), #1566, .T. ) ;
#3021 = CARTESIAN_POINT ( 'NONE',  ( 0.000000000000000000, 0.3464566929133857109, 0.000000000000000000 ) ) ;
#3022 = CARTESIAN_POINT ( 'NONE',  ( -1.965385743026580867, -2.834157585141949820, 0.1664812183409376256 ) ) ;
#3023 = CARTESIAN_POINT ( 'NONE',  ( -1.187759193896365639, 0.3304858427616815253, -0.05905511811023614333 ) ) ;
#3024 = ADVANCED_FACE ( 'NONE', ( #6312, #7437 ), #14429, .F. ) ;
#3025 = CARTESIAN_POINT ( 'NONE',  ( -2.011807227224585493, -2.756102811318750678, -0.1765457041329570320 ) ) ;
#3026 = DIRECTION ( 'NONE',  ( 0.000000000000000000, 0.000000000000000000, 1.000000000000000000 ) ) ;
#3027 = CARTESIAN_POINT ( 'NONE',  ( -0.1023622047242992716, -0.4881889763779528324, -0.2482618547482104143 ) ) ;
#3028 = B_SPLINE_CURVE_WITH_KNOTS ( 'NONE', 3,
 ( #1818, #12644, #11385, #665 ),
 .UNSPECIFIED., .F., .F.,
 ( 4, 4 ),
 ( 0.0009905856238791850652, 0.002309601750613615636 ),
 .UNSPECIFIED. ) ;
#3029 = CARTESIAN_POINT ( 'NONE',  ( 0.1618514667033794374, -0.4921259842519685179, 0.2161887458866224576 ) ) ;
#3030 = CARTESIAN_POINT ( 'NONE',  ( -2.065886881322887447, -2.386349482470467187, -0.1342517337147210998 ) ) ;
#3031 = EDGE_LOOP ( 'NONE', ( #13988, #787, #14571, #12732 ) ) ;
#3032 = ORIENTED_EDGE ( 'NONE', *, *, #5938, .F. ) ;
#3033 = VERTEX_POINT ( 'NONE', #7348 ) ;
#3034 = ORIENTED_EDGE ( 'NONE', *, *, #6840, .F. ) ;
#3035 = EDGE_CURVE ( 'NONE', #880, #14935, #14123, .T. ) ;
#3036 = DIRECTION ( 'NONE',  ( -0.000000000000000000, 1.000000000000000000, -0.000000000000000000 ) ) ;
#3037 = CARTESIAN_POINT ( 'NONE',  ( 0.2330381427387010207, -0.1023622047244094474, 0.06574460052804878551 ) ) ;
#3038 = CARTESIAN_POINT ( 'NONE',  ( 0.4307978335858664853, -0.003937007874015747977, 0.4279391777402732910 ) ) ;
#3039 = ADVANCED_FACE ( 'NONE', ( #5067 ), #2106, .T. ) ;
#3040 = DIRECTION ( 'NONE',  ( -1.000000000000000000, 8.673617379884049672E-15, 0.000000000000000000 ) ) ;
#3041 = LINE ( 'NONE', #4136, #5588 ) ;
#3042 = EDGE_CURVE ( 'NONE', #13421, #8067, #855, .T. ) ;
#3043 = LINE ( 'NONE', #704, #14660 ) ;
#3044 = DIRECTION ( 'NONE',  ( 0.000000000000000000, 0.000000000000000000, 1.000000000000000000 ) ) ;
#3045 = DIRECTION ( 'NONE',  ( 0.8144815189573203495, -0.5801894994542524664, 0.000000000000000000 ) ) ;
#3046 = CARTESIAN_POINT ( 'NONE',  ( -0.3478321452968090588, -0.2952755905511811330, 0.3144726105131496752 ) ) ;
#3047 = ORIENTED_EDGE ( 'NONE', *, *, #11140, .T. ) ;
#3048 = DIRECTION ( 'NONE',  ( -1.000000000000000000, 1.224646799147361096E-16, 0.000000000000000000 ) ) ;
#3049 = VERTEX_POINT ( 'NONE', #5153 ) ;
#3050 = EDGE_LOOP ( 'NONE', ( #4973, #14863, #1563, #9783 ) ) ;
#3051 = EDGE_LOOP ( 'NONE', ( #5544, #7656, #320, #1336 ) ) ;
#3052 = AXIS2_PLACEMENT_3D ( 'NONE', #2295, #14057, #9447 ) ;
#3053 = CARTESIAN_POINT ( 'NONE',  ( -1.181102362204724310, 0.1279527559055117225, 0.02559055118110236185 ) ) ;
#3054 = CARTESIAN_POINT ( 'NONE',  ( 0.000000000000000000, 0.000000000000000000, 0.000000000000000000 ) ) ;
#3055 = DIRECTION ( 'NONE',  ( 0.000000000000000000, 0.000000000000000000, -1.000000000000000000 ) ) ;
#3056 = SPHERICAL_SURFACE ( 'NONE', #7459, 0.003937007874015747977 ) ;
#3057 = CARTESIAN_POINT ( 'NONE',  ( -1.181845651246067774, 0.3414517841026233902, -0.04963174987412501821 ) ) ;
#3058 = VERTEX_POINT ( 'NONE', #1421 ) ;
#3059 = DIRECTION ( 'NONE',  ( -0.000000000000000000, -1.000000000000000000, -0.000000000000000000 ) ) ;
#3060 = CARTESIAN_POINT ( 'NONE',  ( -0.1181102362204724532, 2.637795275590551825, 0.03937007874015747977 ) ) ;
#3061 = FACE_OUTER_BOUND ( 'NONE', #11521, .T. ) ;
#3062 = CARTESIAN_POINT ( 'NONE',  ( -0.5452755905511542656, -0.1023622047244094474, 0.2375319020879049503 ) ) ;
#3063 = ORIENTED_EDGE ( 'NONE', *, *, #12522, .T. ) ;
#3064 = CARTESIAN_POINT ( 'NONE',  ( 0.000000000000000000, 1.338582677165354395, 0.000000000000000000 ) ) ;
#3065 = ORIENTED_EDGE ( 'NONE', *, *, #8994, .T. ) ;
#3066 = EDGE_LOOP ( 'NONE', ( #13051, #11162, #10572, #6574 ) ) ;
#3067 = DIRECTION ( 'NONE',  ( -1.000000000000000000, 0.000000000000000000, 0.000000000000000000 ) ) ;
#3068 = PLANE ( 'NONE',  #14667 ) ;
#3069 = CYLINDRICAL_SURFACE ( 'NONE', #9359, 2.795275590551181466 ) ;
#3070 = DIRECTION ( 'NONE',  ( 0.8660254037844383745, 0.000000000000000000, -0.5000000000000004441 ) ) ;
#3071 = CARTESIAN_POINT ( 'NONE',  ( -0.2364476915723336681, -0.4921259842519685179, 0.06377609659094583827 ) ) ;
#3072 = AXIS2_PLACEMENT_3D ( 'NONE', #10554, #11816, #1081 ) ;
#3073 = EDGE_CURVE ( 'NONE', #14806, #2402, #6094, .T. ) ;
#3074 = CARTESIAN_POINT ( 'NONE',  ( 0.5452492930724234244, 1.338582677165354395, 0.2466088494548705212 ) ) ;
#3075 = ORIENTED_EDGE ( 'NONE', *, *, #11980, .T. ) ;
#3076 = CARTESIAN_POINT ( 'NONE',  ( 0.000000000000000000, 0.5826771653543306728, 0.000000000000000000 ) ) ;
#3077 = AXIS2_PLACEMENT_3D ( 'NONE', #2323, #8225, #12997 ) ;
#3078 = DIRECTION ( 'NONE',  ( -0.8011800915434522663, 0.5984233124757303290, 0.000000000000000000 ) ) ;
#3079 = AXIS2_PLACEMENT_3D ( 'NONE', #8502, #11969, #1232 ) ;
#3080 = DIRECTION ( 'NONE',  ( 0.000000000000000000, 1.000000000000000000, -0.000000000000000000 ) ) ;
#3081 = ADVANCED_FACE ( 'NONE', ( #12691 ), #10858, .T. ) ;
#3082 =( BOUNDED_CURVE ( )  B_SPLINE_CURVE ( 3, ( #11345, #10320, #4223, #9012 ),
 .UNSPECIFIED., .F., .T. ) 
 B_SPLINE_CURVE_WITH_KNOTS ( ( 4, 4 ),
 ( 4.182272261879897535, 4.712388980384695003 ),
 .UNSPECIFIED. ) 
 CURVE ( )  GEOMETRIC_REPRESENTATION_ITEM ( )  RATIONAL_B_SPLINE_CURVE ( ( 1.000000000000000000, 0.9767181429391975644, 0.9767181429391975644, 1.000000000000000000 ) ) 
 REPRESENTATION_ITEM ( '' )  );
#3083 = DIRECTION ( 'NONE',  ( 0.000000000000000000, 0.000000000000000000, 1.000000000000000000 ) ) ;
#3084 = ORIENTED_EDGE ( 'NONE', *, *, #6925, .T. ) ;
#3085 = EDGE_LOOP ( 'NONE', ( #12830, #8018, #6164 ) ) ;
#3087 = EDGE_LOOP ( 'NONE', ( #1035, #8598, #3983, #300 ) ) ;
#3086 = AXIS2_PLACEMENT_3D ( 'NONE', #5008, #9805, #536 ) ;
#3088 = CIRCLE ( 'NONE', #5821, 0.1279527559055117780 ) ;
#3089 = ORIENTED_EDGE ( 'NONE', *, *, #5220, .T. ) ;
#3090 = AXIS2_PLACEMENT_3D ( 'NONE', #10434, #14910, #14032 ) ;
#3091 = CIRCLE ( 'NONE', #13849, 0.6614173228346456046 ) ;
#3092 = EDGE_CURVE ( 'NONE', #14773, #1163, #12868, .T. ) ;
#3093 = PLANE ( 'NONE',  #9616 ) ;
#3094 = CARTESIAN_POINT ( 'NONE',  ( -2.003349645206483842, -2.780432114833338630, 0.1578450787283683932 ) ) ;
#3095 = EDGE_CURVE ( 'NONE', #12818, #15326, #8617, .T. ) ;
#3096 = DIRECTION ( 'NONE',  ( 0.8660254037844387076, 0.000000000000000000, -0.4999999999999998890 ) ) ;
#3097 = CARTESIAN_POINT ( 'NONE',  ( -1.969039959700434217, -2.872969167378714772, -0.1271901138548807708 ) ) ;
#3098 = CARTESIAN_POINT ( 'NONE',  ( -0.2681506793016945611, -0.4881889763779528324, 0.03207310886158504931 ) ) ;
#3099 = AXIS2_PLACEMENT_3D ( 'NONE', #10851, #8437, #14397 ) ;
#3100 = CIRCLE ( 'NONE', #15110, 1.885039370078740451 ) ;
#3101 = DIRECTION ( 'NONE',  ( -0.9966420383350279577, 0.000000000000000000, -0.08188191145424326967 ) ) ;
#3102 = AXIS2_PLACEMENT_3D ( 'NONE', #11499, #6865, #9003 ) ;
#3103 = EDGE_CURVE ( 'NONE', #8494, #12201, #11615, .T. ) ;
#3104 = CARTESIAN_POINT ( 'NONE',  ( 0.06299212598430639631, -0.1023622047244094474, -0.5870514566507987197 ) ) ;
#3105 = CARTESIAN_POINT ( 'NONE',  ( -2.107119091007230605, -2.011924609756351678, -0.1111957386528079073 ) ) ;
#3106 = CIRCLE ( 'NONE', #6335, 0.003937007874015724558 ) ;
#3107 = ADVANCED_FACE ( 'NONE', ( #11577 ), #4609, .F. ) ;
#3108 = AXIS2_PLACEMENT_3D ( 'NONE', #11941, #12791, #9339 ) ;
#3109 = ORIENTED_EDGE ( 'NONE', *, *, #1959, .T. ) ;
#3110 = EDGE_LOOP ( 'NONE', ( #14017, #11204, #4700 ) ) ;
#3111 = EDGE_LOOP ( 'NONE', ( #6752, #5298, #6491, #14803 ) ) ;
#3112 = ORIENTED_EDGE ( 'NONE', *, *, #2035, .F. ) ;
#3113 = AXIS2_PLACEMENT_3D ( 'NONE', #2014, #11334, #6542 ) ;
#3114 = AXIS2_PLACEMENT_3D ( 'NONE', #12038, #13350, #14535 ) ;
#3115 = CIRCLE ( 'NONE', #13873, 0.5511811023622046335 ) ;
#3116 = CARTESIAN_POINT ( 'NONE',  ( -2.163017314575554462, -1.630597114118274238, -0.1033464566929129386 ) ) ;
#3117 = CARTESIAN_POINT ( 'NONE',  ( -1.181102362204724310, 0.1279527559055117225, 0.02952755905511811330 ) ) ;
#3118 = TOROIDAL_SURFACE ( 'NONE', #13385, 0.04330708661417328326, 0.003937007874015747977 ) ;
#3119 = CARTESIAN_POINT ( 'NONE',  ( 0.1724006475077544120, -0.4881889763779528324, 0.1768186671464649640 ) ) ;
#3120 = AXIS2_PLACEMENT_3D ( 'NONE', #14831, #8886, #2932 ) ;
#3121 = DIRECTION ( 'NONE',  ( 0.8660254037844400399, -0.000000000000000000, 0.4999999999999976130 ) ) ;
#3122 = CARTESIAN_POINT ( 'NONE',  ( 0.4749369078591172411, -0.4881889763779528324, 0.3514880584999470203 ) ) ;
#3123 = DIRECTION ( 'NONE',  ( 0.000000000000000000, 1.000000000000000000, -0.000000000000000000 ) ) ;
#3124 = EDGE_LOOP ( 'NONE', ( #551, #8769, #10127, #3337 ) ) ;
#3125 = DIRECTION ( 'NONE',  ( -0.000000000000000000, -1.000000000000000000, -0.000000000000000000 ) ) ;
#3126 = EDGE_CURVE ( 'NONE', #10243, #2898, #9355, .T. ) ;
#3127 = VECTOR ( 'NONE', #9816, 39.37007874015748143 ) ;
#3128 = VERTEX_POINT ( 'NONE', #6718 ) ;
#3129 = VERTEX_POINT ( 'NONE', #7816 ) ;
#3130 = AXIS2_PLACEMENT_3D ( 'NONE', #8857, #1734, #13726 ) ;
#3131 = ADVANCED_FACE ( 'NONE', ( #12607 ), #1862, .T. ) ;
#3132 = PRODUCT_DEFINITION_CONTEXT ( 'detailed design', #14004, 'design' ) ;
#3133 = EDGE_LOOP ( 'NONE', ( #9123, #10954, #516, #9048 ) ) ;
#3134 = CARTESIAN_POINT ( 'NONE',  ( -0.6692913385826770867, 0.5511811023622046335, 0.000000000000000000 ) ) ;
#3135 = VECTOR ( 'NONE', #1663, 39.37007874015748143 ) ;
#3136 = AXIS2_PLACEMENT_3D ( 'NONE', #2818, #2916, #9975 ) ;
#3137 = AXIS2_PLACEMENT_3D ( 'NONE', #7532, #6267, #208 ) ;
#3138 = FACE_OUTER_BOUND ( 'NONE', #609, .T. ) ;
#3139 = DIRECTION ( 'NONE',  ( -1.000000000000000000, 0.000000000000000000, 0.000000000000000000 ) ) ;
#3140 = FACE_OUTER_BOUND ( 'NONE', #12503, .T. ) ;
#3141 = AXIS2_PLACEMENT_3D ( 'NONE', #14247, #3347, #10485 ) ;
#3142 = DIRECTION ( 'NONE',  ( 0.000000000000000000, -1.000000000000000000, 0.000000000000000000 ) ) ;
#3143 = ORIENTED_EDGE ( 'NONE', *, *, #8258, .F. ) ;
#3144 = DIRECTION ( 'NONE',  ( 1.000000000000000000, 0.000000000000000000, 0.000000000000000000 ) ) ;
#3145 = CARTESIAN_POINT ( 'NONE',  ( 0.000000000000000000, 0.5433070866141731514, 0.000000000000000000 ) ) ;
#3146 = CARTESIAN_POINT ( 'NONE',  ( -0.002345674784311424250, -0.1605320876855827750, -0.0006089964461715403551 ) ) ;
#3147 = CARTESIAN_POINT ( 'NONE',  ( -1.431036756819011213, -0.02829858486107887303, -0.07874015748031495954 ) ) ;
#3148 = EDGE_LOOP ( 'NONE', ( #14254, #14639, #983, #6575, #5807, #13066 ) ) ;
#3149 = CARTESIAN_POINT ( 'NONE',  ( 1.181102362204724310, 4.044111181948214319E-16, -0.02952755905511811330 ) ) ;
#3150 = VECTOR ( 'NONE', #2641, 39.37007874015748143 ) ;
#3151 = AXIS2_PLACEMENT_3D ( 'NONE', #2075, #1159, #5819 ) ;
#3152 = VECTOR ( 'NONE', #2733, 39.37007874015748143 ) ;
#3153 = ORIENTED_EDGE ( 'NONE', *, *, #5609, .F. ) ;
#3154 = EDGE_CURVE ( 'NONE', #10586, #8715, #9112, .T. ) ;
#3155 = ORIENTED_EDGE ( 'NONE', *, *, #1076, .F. ) ;
#3156 = VECTOR ( 'NONE', #5997, 39.37007874015748143 ) ;
#3157 = VERTEX_POINT ( 'NONE', #10255 ) ;
#3158 = CYLINDRICAL_SURFACE ( 'NONE', #2819, 0.03937007874015747977 ) ;
#3159 = CARTESIAN_POINT ( 'NONE',  ( -0.5511811023622046335, 1.417322834645669438, 0.000000000000000000 ) ) ;
#3160 = CARTESIAN_POINT ( 'NONE',  ( -0.02636306718620661307, 0.1724112960300225594, -0.0009221601458012943170 ) ) ;
#3161 = DIRECTION ( 'NONE',  ( 0.5000000000000069944, -7.511572993685774449E-15, -0.8660254037844347108 ) ) ;
#3162 = DIRECTION ( 'NONE',  ( 0.000000000000000000, 0.000000000000000000, -1.000000000000000000 ) ) ;
#3163 = AXIS2_PLACEMENT_3D ( 'NONE', #8803, #4184, #3083 ) ;
#3164 = DIRECTION ( 'NONE',  ( 0.000000000000000000, 0.000000000000000000, 1.000000000000000000 ) ) ;
#3165 = VERTEX_POINT ( 'NONE', #1796 ) ;
#3166 = CARTESIAN_POINT ( 'NONE',  ( 1.880363195541211833E-17, 2.161417322834645827, -0.1535433070866141780 ) ) ;
#3167 = CARTESIAN_POINT ( 'NONE',  ( 0.1259842519685039353, 2.440944881889763884, 0.04724409448818898266 ) ) ;
#3168 = CARTESIAN_POINT ( 'NONE',  ( -1.181342415325333350, 0.3435647566446739520, -0.03937007874015747977 ) ) ;
#3169 = TOROIDAL_SURFACE ( 'NONE', #3425, 0.2303149606299203511, 0.01968503937007873988 ) ;
#3170 = CARTESIAN_POINT ( 'NONE',  ( 0.4859532342797860394, 1.338582677165354395, 0.3487562073009374264 ) ) ;
#3171 = VERTEX_POINT ( 'NONE', #14971 ) ;
#3172 = EDGE_LOOP ( 'NONE', ( #4781, #1747, #6330, #11606 ) ) ;
#3173 = CARTESIAN_POINT ( 'NONE',  ( 0.3746568166374371622, -0.2952755905511811330, 0.1026565861461821993 ) ) ;
#3174 = ORIENTED_EDGE ( 'NONE', *, *, #4138, .F. ) ;
#3175 = CIRCLE ( 'NONE', #14690, 0.003937007874015721089 ) ;
#3176 = EDGE_CURVE ( 'NONE', #13376, #14592, #13785, .T. ) ;
#3177 = ORIENTED_EDGE ( 'NONE', *, *, #9761, .F. ) ;
#3178 = AXIS2_PLACEMENT_3D ( 'NONE', #416, #11284, #7595 ) ;
#3179 = EDGE_CURVE ( 'NONE', #13620, #5863, #3082, .T. ) ;
#3180 = CARTESIAN_POINT ( 'NONE',  ( -0.07874015748031544526, -0.1771653543307084577, -0.05905511811023622659 ) ) ;
#3181 = DIRECTION ( 'NONE',  ( 0.000000000000000000, 0.000000000000000000, -1.000000000000000000 ) ) ;
#3182 = AXIS2_PLACEMENT_3D ( 'NONE', #10293, #813, #7003 ) ;
#3183 = CARTESIAN_POINT ( 'NONE',  ( 8.582170482213735190E-17, 1.385826771653543510, -0.7007874015748031260 ) ) ;
#3184 =( BOUNDED_CURVE ( )  B_SPLINE_CURVE ( 3, ( #8377, #3453, #11922, #2427 ),
 .UNSPECIFIED., .F., .T. ) 
 B_SPLINE_CURVE_WITH_KNOTS ( ( 4, 4 ),
 ( 4.712388980384689674, 6.283185307179586232 ),
 .UNSPECIFIED. ) 
 CURVE ( )  GEOMETRIC_REPRESENTATION_ITEM ( )  RATIONAL_B_SPLINE_CURVE ( ( 1.000000000000000000, 0.8047378541243649375, 0.8047378541243649375, 1.000000000000000000 ) ) 
 REPRESENTATION_ITEM ( '' )  );
#3185 = VECTOR ( 'NONE', #3045, 39.37007874015748854 ) ;
#3186 = CARTESIAN_POINT ( 'NONE',  ( -0.1657884745773953450, -0.4921259842519685179, 0.2093696482190284258 ) ) ;
#3187 = VECTOR ( 'NONE', #14797, 39.37007874015748143 ) ;
#3188 = CARTESIAN_POINT ( 'NONE',  ( -0.3314531923919099565, -0.2952755905511811330, 0.2641016316388978824 ) ) ;
#3189 = CARTESIAN_POINT ( 'NONE',  ( -2.107032438837129096, -1.725900680217038463, -0.1037380524286266731 ) ) ;
#3190 = CIRCLE ( 'NONE', #13204, 0.1653543307086614012 ) ;
#3191 = ORIENTED_EDGE ( 'NONE', *, *, #1306, .T. ) ;
#3192 = ORIENTED_EDGE ( 'NONE', *, *, #3960, .F. ) ;
#3193 = EDGE_CURVE ( 'NONE', #675, #10534, #10625, .T. ) ;
#3194 = CIRCLE ( 'NONE', #2443, 0.007874015748031516770 ) ;
#3195 = ORIENTED_EDGE ( 'NONE', *, *, #4032, .F. ) ;
#3196 = EDGE_CURVE ( 'NONE', #3157, #1093, #4348, .T. ) ;
#3197 = ORIENTED_EDGE ( 'NONE', *, *, #3938, .T. ) ;
#3198 = AXIS2_PLACEMENT_3D ( 'NONE', #4579, #9368, #8203 ) ;
#3199 = EDGE_CURVE ( 'NONE', #8242, #11793, #15430, .T. ) ;
#3200 = CARTESIAN_POINT ( 'NONE',  ( -1.590143285778936821, 0.1215581459426987310, -0.06156531251049104925 ) ) ;
#3201 = DIRECTION ( 'NONE',  ( 0.000000000000000000, -0.000000000000000000, -1.000000000000000000 ) ) ;
#3202=STYLED_ITEM('',(#15519),#14611);
#3203 = SPHERICAL_SURFACE ( 'NONE', #8688, 0.003937007874015747977 ) ;
#3204 = DIRECTION ( 'NONE',  ( -0.000000000000000000, 1.000000000000000000, -0.000000000000000000 ) ) ;
#3205 = DIRECTION ( 'NONE',  ( 0.5000000000000004441, -0.000000000000000000, -0.8660254037844384856 ) ) ;
#3206 = DIRECTION ( 'NONE',  ( -0.000000000000000000, -1.000000000000000000, 4.956352788505160310E-16 ) ) ;
#3207 = CARTESIAN_POINT ( 'NONE',  ( -0.5871416322685659717, -0.09448818897637796532, 0.1610807828475335490 ) ) ;
#3208 = ORIENTED_EDGE ( 'NONE', *, *, #7006, .F. ) ;
#3209 = DIRECTION ( 'NONE',  ( 0.000000000000000000, -1.000000000000000000, -0.000000000000000000 ) ) ;
#3210 = DIRECTION ( 'NONE',  ( -1.224646799147353700E-16, 0.000000000000000000, -1.000000000000000000 ) ) ;
#3211 = CIRCLE ( 'NONE', #4957, 0.003937007874015754916 ) ;
#3212 = ORIENTED_EDGE ( 'NONE', *, *, #15142, .F. ) ;
#3213 = VERTEX_POINT ( 'NONE', #5 ) ;
#3214 = AXIS2_PLACEMENT_3D ( 'NONE', #13541, #5230, #2804 ) ;
#3215 = ADVANCED_FACE ( 'NONE', ( #2189 ), #13112, .T. ) ;
#3216 = EDGE_LOOP ( 'NONE', ( #1317, #899, #14404, #4350 ) ) ;
#3217 = B_SPLINE_CURVE_WITH_KNOTS ( 'NONE', 3,
 ( #10880, #14495, #2428, #9558, #9643, #2736 ),
 .UNSPECIFIED., .F., .F.,
 ( 4, 2, 4 ),
 ( 0.000000000000000000, 0.0001791382075655885420, 0.0003582764151311770839 ),
 .UNSPECIFIED. ) ;
#3218 = FACE_OUTER_BOUND ( 'NONE', #8324, .T. ) ;
#3219 = EDGE_CURVE ( 'NONE', #1302, #11324, #3106, .T. ) ;
#3220 = DIRECTION ( 'NONE',  ( 0.000000000000000000, 0.000000000000000000, -1.000000000000000000 ) ) ;
#3221 = CARTESIAN_POINT ( 'NONE',  ( 0.06692913385832212347, -0.4881889763779528324, -0.5909884645248143498 ) ) ;
#3222 = AXIS2_PLACEMENT_3D ( 'NONE', #4503, #11730, #15317 ) ;
#3223 = FACE_OUTER_BOUND ( 'NONE', #13130, .T. ) ;
#3224 = FACE_OUTER_BOUND ( 'NONE', #7501, .T. ) ;
#3225 = ORIENTED_EDGE ( 'NONE', *, *, #14489, .F. ) ;
#3226 = DIRECTION ( 'NONE',  ( 0.000000000000000000, 0.000000000000000000, -1.000000000000000000 ) ) ;
#3227 = EDGE_CURVE ( 'NONE', #11994, #6744, #14175, .T. ) ;
#3228 = CARTESIAN_POINT ( 'NONE',  ( -0.7086614173228346081, 1.653543307086614567, 0.000000000000000000 ) ) ;
#3229 = CARTESIAN_POINT ( 'NONE',  ( 0.5433070866142283295, -0.4921259842519685179, 0.2409414509217496780 ) ) ;
#3230 = FACE_OUTER_BOUND ( 'NONE', #1118, .T. ) ;
#3231 = ORIENTED_EDGE ( 'NONE', *, *, #4376, .T. ) ;
#3232 = CARTESIAN_POINT ( 'NONE',  ( 0.09061599198715353243, 0.07874015748031495954, 0.007444810018878659542 ) ) ;
#3233 = EDGE_LOOP ( 'NONE', ( #15290, #6615, #1483, #1500 ) ) ;
#3234 = ORIENTED_EDGE ( 'NONE', *, *, #7923, .F. ) ;
#3235 = EDGE_CURVE ( 'NONE', #2210, #7634, #3850, .T. ) ;
#3236 = FACE_BOUND ( 'NONE', #9146, .T. ) ;
#3237 = CARTESIAN_POINT ( 'NONE',  ( 0.09842519685044806566, -0.4881889763779528324, -0.2482618547481154347 ) ) ;
#3238 = CARTESIAN_POINT ( 'NONE',  ( -0.03726199245316209885, 0.1489178558048124545, -0.04781523662143043890 ) ) ;
#3239 = LINE ( 'NONE', #11294, #15113 ) ;
#3240 = ITEM_DEFINED_TRANSFORMATION ( 'NONE', 'NONE', #619,  #11481 ) ;
#3241 = CARTESIAN_POINT ( 'NONE',  ( 0.2762316197870728907, -0.2952755905511811330, 0.2731340278359848384 ) ) ;
#3242 = CARTESIAN_POINT ( 'NONE',  ( 0.06692913385832209572, -0.4921259842519685179, -0.2377126739437405434 ) ) ;
#3243 = ORIENTED_EDGE ( 'NONE', *, *, #14484, .F. ) ;
#3244 = DIRECTION ( 'NONE',  ( 0.8660254037844385966, 0.000000000000000000, 0.5000000000000001110 ) ) ;
#3245 = EDGE_CURVE ( 'NONE', #11911, #14594, #14083, .T. ) ;
#3246 = LINE ( 'NONE', #12797, #13380 ) ;
#3247 = CARTESIAN_POINT ( 'NONE',  ( -0.7086614173228346081, 0.5905511811023621549, 0.000000000000000000 ) ) ;
#3248 = FILL_AREA_STYLE ('',( #13983 ) ) ;
#3249 = ORIENTED_EDGE ( 'NONE', *, *, #14299, .F. ) ;
#3250 = ORIENTED_EDGE ( 'NONE', *, *, #7324, .T. ) ;
#3251 = CARTESIAN_POINT ( 'NONE',  ( 0.5452492930724234244, 1.043307086614173373, 0.2466088494548703824 ) ) ;
#3252 = ORIENTED_EDGE ( 'NONE', *, *, #15255, .F. ) ;
#3253 = ORIENTED_EDGE ( 'NONE', *, *, #14977, .T. ) ;
#3254 = ORIENTED_EDGE ( 'NONE', *, *, #14337, .F. ) ;
#3255 = CARTESIAN_POINT ( 'NONE',  ( 0.4307978335858663188, 0.000000000000000000, 0.4279391777402732910 ) ) ;
#3256 = CARTESIAN_POINT ( 'NONE',  ( -2.077672400517819984, -2.160918623940574879, -0.09867007254763489332 ) ) ;
#3257 = CARTESIAN_POINT ( 'NONE',  ( 6.750021727583836750E-17, 0.5590551181102362266, 0.5511811023622046335 ) ) ;
#3258 = FACE_OUTER_BOUND ( 'NONE', #6830, .T. ) ;
#3259 = DIRECTION ( 'NONE',  ( -0.8660254037844308250, 0.000000000000000000, 0.5000000000000134337 ) ) ;
#3260 = CARTESIAN_POINT ( 'NONE',  ( -0.06011003619056348030, -0.09842519685039370636, -0.2337756660698198097 ) ) ;
#3261 = CARTESIAN_POINT ( 'NONE',  ( 0.5484644751328278112, 0.000000000000000000, 0.2393730054594799261 ) ) ;
#3262 = ORIENTED_EDGE ( 'NONE', *, *, #1764, .T. ) ;
#3263 = ORIENTED_EDGE ( 'NONE', *, *, #8404, .T. ) ;
#3264 = EDGE_LOOP ( 'NONE', ( #1021, #4368, #6682, #3063 ) ) ;
#3265 = ORIENTED_EDGE ( 'NONE', *, *, #6677, .T. ) ;
#3266 = DIRECTION ( 'NONE',  ( -0.000000000000000000, -0.000000000000000000, -1.000000000000000000 ) ) ;
#3267 = LINE ( 'NONE', #2087, #1657 ) ;
#3268 = CARTESIAN_POINT ( 'NONE',  ( -0.004432333661850347203, 0.1530140478774274504, 0.007791225829902534428 ) ) ;
#3269 = EDGE_CURVE ( 'NONE', #7658, #10513, #8288, .T. ) ;
#3270 = PLANE ( 'NONE',  #4356 ) ;
#3271 = CARTESIAN_POINT ( 'NONE',  ( 0.000000000000000000, 0.4133858267716535306, 0.000000000000000000 ) ) ;
#3272 = CARTESIAN_POINT ( 'NONE',  ( 0.000000000000000000, 0.3149606299212598381, 0.7007874015748031260 ) ) ;
#3273 = CARTESIAN_POINT ( 'NONE',  ( -1.941812372403446618, -2.756696258605407568, -0.1575938902943630204 ) ) ;
#3274 = ADVANCED_FACE ( 'NONE', ( #10722, #1176 ), #9395, .F. ) ;
#3275 = ORIENTED_EDGE ( 'NONE', *, *, #9898, .F. ) ;
#3276 = CARTESIAN_POINT ( 'NONE',  ( 0.4861941749621881415, 1.043307086614173373, 0.3488953144687809704 ) ) ;
#3277 = CARTESIAN_POINT ( 'NONE',  ( 0.000000000000000000, 0.3149606299212598381, 0.5984251968503937480 ) ) ;
#3278 = ORIENTED_EDGE ( 'NONE', *, *, #4424, .T. ) ;
#3279 = B_SPLINE_CURVE_WITH_KNOTS ( 'NONE', 3,
 ( #10224, #3170, #8895, #3012 ),
 .UNSPECIFIED., .F., .F.,
 ( 4, 4 ),
 ( 0.000000000000000000, 2.119993237936537351E-05 ),
 .UNSPECIFIED. ) ;
#3280 = EDGE_CURVE ( 'NONE', #13379, #579, #574, .T. ) ;
#3281 = ORIENTED_EDGE ( 'NONE', *, *, #11999, .T. ) ;
#3282 = ORIENTED_EDGE ( 'NONE', *, *, #12364, .F. ) ;
#3283 = CARTESIAN_POINT ( 'NONE',  ( -0.5511811023622046335, 2.401574803149606918, 0.000000000000000000 ) ) ;
#3284 = EDGE_CURVE ( 'NONE', #11649, #3451, #9838, .T. ) ;
#3285 = CYLINDRICAL_SURFACE ( 'NONE', #7113, 0.003937007874015758385 ) ;
#3286 = CARTESIAN_POINT ( 'NONE',  ( -1.950247696211656612, -2.878813950563311685, 0.1420638311955204902 ) ) ;
#3287 = CARTESIAN_POINT ( 'NONE',  ( -1.293236445124221312, 0.1355266887446167634, 0.03937007874015747977 ) ) ;
#3288 = CARTESIAN_POINT ( 'NONE',  ( 0.1552072824047652233, -0.09448818897637796532, -0.5870514566507987197 ) ) ;
#3289 = DIRECTION ( 'NONE',  ( -0.8144815189573204606, 0.5801894994542525774, 1.283760644411384396E-16 ) ) ;
#3290 = EDGE_CURVE ( 'NONE', #2262, #15003, #7076, .T. ) ;
#3291 = ORIENTED_EDGE ( 'NONE', *, *, #11119, .F. ) ;
#3292 = APPLICATION_CONTEXT ( 'automotive_design' ) ;
#3293 = DIRECTION ( 'NONE',  ( -1.000000000000000000, 0.000000000000000000, 0.000000000000000000 ) ) ;
#3294 = CYLINDRICAL_SURFACE ( 'NONE', #8865, 0.05905511811023625435 ) ;
#3295 = CARTESIAN_POINT ( 'NONE',  ( -0.01783696211247719210, 0.1513009196653194999, 0.03097470637416573427 ) ) ;
#3296 = LINE ( 'NONE', #730, #1589 ) ;
#3297 = ORIENTED_EDGE ( 'NONE', *, *, #3431, .F. ) ;
#3298 = ADVANCED_FACE ( 'NONE', ( #4983 ), #12280, .T. ) ;
#3299 = CARTESIAN_POINT ( 'NONE',  ( 0.4861941749621881415, 1.338582677165354395, 0.3488953144687809704 ) ) ;
#3300 = ORIENTED_EDGE ( 'NONE', *, *, #2672, .T. ) ;
#3301 = B_SPLINE_CURVE_WITH_KNOTS ( 'NONE', 3,
 ( #8539, #11263, #7892, #13315, #14872 ),
 .UNSPECIFIED., .F., .F.,
 ( 4, 1, 4 ),
 ( 2.212246760591329979E-07, 0.001154921763055310720, 0.002309622301434562531 ),
 .UNSPECIFIED. ) ;
#3302 = EDGE_LOOP ( 'NONE', ( #832, #3932, #4443, #14506, #735, #1112 ) ) ;
#3303 = ORIENTED_EDGE ( 'NONE', *, *, #12800, .T. ) ;
#3304 = CARTESIAN_POINT ( 'NONE',  ( 0.000000000000000000, 2.161417322834645827, 0.000000000000000000 ) ) ;
#3305 = DIRECTION ( 'NONE',  ( 0.000000000000000000, 1.000000000000000000, -0.000000000000000000 ) ) ;
#3306 = DIRECTION ( 'NONE',  ( 0.5000000000000001110, 0.000000000000000000, 0.8660254037844385966 ) ) ;
#3307 = CARTESIAN_POINT ( 'NONE',  ( -0.07874015748031543138, -0.1682792322177920907, -0.03937007874015747977 ) ) ;
#3308 = APPLICATION_PROTOCOL_DEFINITION ( 'draft international standard', 'automotive_design', 1998, #7577 ) ;
#3309 = DIRECTION ( 'NONE',  ( 0.000000000000000000, 0.000000000000000000, 1.000000000000000000 ) ) ;
#3310 = CARTESIAN_POINT ( 'NONE',  ( -0.02433043306709230594, -0.1808586691373950950, 0.01162756877077189034 ) ) ;
#3311 = ORIENTED_EDGE ( 'NONE', *, *, #2713, .T. ) ;
#3312 = CARTESIAN_POINT ( 'NONE',  ( -0.1259842519685039353, 2.440944881889763884, 0.04724409448818898266 ) ) ;
#3313 = CARTESIAN_POINT ( 'NONE',  ( -1.574484809660414042, 0.1100025355989073528, 0.06175692796217682051 ) ) ;
#3314 = EDGE_CURVE ( 'NONE', #2187, #6409, #9780, .T. ) ;
#3315 = EDGE_LOOP ( 'NONE', ( #6806, #8194, #8052, #694, #6743, #3591 ) ) ;
#3316 = ORIENTED_EDGE ( 'NONE', *, *, #14821, .F. ) ;
#3317 = CARTESIAN_POINT ( 'NONE',  ( 0.5447670804913020692, 1.043292445042268257, 0.2463304438913534455 ) ) ;
#3318 = ORIENTED_EDGE ( 'NONE', *, *, #11031, .F. ) ;
#3319 = ORIENTED_EDGE ( 'NONE', *, *, #714, .F. ) ;
#3320 = ADVANCED_FACE ( 'NONE', ( #1398 ), #3746, .T. ) ;
#3321 = ORIENTED_EDGE ( 'NONE', *, *, #11441, .T. ) ;
#3322 = DIRECTION ( 'NONE',  ( -0.000000000000000000, 1.000000000000000000, 0.000000000000000000 ) ) ;
#3323 = AXIS2_PLACEMENT_3D ( 'NONE', #1951, #6713, #11504 ) ;
#3324 = AXIS2_PLACEMENT_3D ( 'NONE', #4436, #5591, #4856 ) ;
#3325 = DIRECTION ( 'NONE',  ( -0.8660254037844482555, -0.000000000000000000, -0.4999999999999837907 ) ) ;
#3326 = FACE_OUTER_BOUND ( 'NONE', #2874, .T. ) ;
#3327 = LINE ( 'NONE', #8269, #5630 ) ;
#3328 = DIRECTION ( 'NONE',  ( -0.5000000000000209832, 0.000000000000000000, -0.8660254037844266062 ) ) ;
#3329 = CARTESIAN_POINT ( 'NONE',  ( -1.491640810881974977, 0.2222636556240916994, -0.05905511811023622659 ) ) ;
#3330 = CARTESIAN_POINT ( 'NONE',  ( -2.090051324975654268, -1.858423098536573503, -0.08664193191035729491 ) ) ;
#3331 = AXIS2_PLACEMENT_3D ( 'NONE', #2968, #7736, #12525 ) ;
#3332 = CIRCLE ( 'NONE', #8584, 0.003937007874015746242 ) ;
#3333 = ORIENTED_EDGE ( 'NONE', *, *, #7051, .T. ) ;
#3334 = AXIS2_PLACEMENT_3D ( 'NONE', #9692, #14536, #4810 ) ;
#3335 = VERTEX_POINT ( 'NONE', #8590 ) ;
#3336 = AXIS2_PLACEMENT_3D ( 'NONE', #11736, #15322, #1791 ) ;
#3337 = ORIENTED_EDGE ( 'NONE', *, *, #5954, .T. ) ;
#3338 = ORIENTED_EDGE ( 'NONE', *, *, #10463, .F. ) ;
#3339 = PRODUCT_DEFINITION ( 'UNKNOWN', '', #5596, #3132 ) ;
#3340 = DIRECTION ( 'NONE',  ( 0.000000000000000000, -1.000000000000000000, 2.198945251238206020E-16 ) ) ;
#3341 = DIRECTION ( 'NONE',  ( 0.000000000000000000, 0.000000000000000000, -1.000000000000000000 ) ) ;
#3342 = CIRCLE ( 'NONE', #9859, 0.6692913385826770867 ) ;
#3343 = CARTESIAN_POINT ( 'NONE',  ( 0.2796411686208698510, -0.2952755905511811330, 0.2751025317729927644 ) ) ;
#3344 = CARTESIAN_POINT ( 'NONE',  ( -0.08151194962748878337, 0.1637246173173400321, 0.05905511811023621965 ) ) ;
#3345 = VECTOR ( 'NONE', #5304, 39.37007874015748854 ) ;
#3346 = FACE_OUTER_BOUND ( 'NONE', #4239, .T. ) ;
#3347 = DIRECTION ( 'NONE',  ( 0.000000000000000000, -1.000000000000000000, 0.000000000000000000 ) ) ;
#3348 = AXIS2_PLACEMENT_3D ( 'NONE', #5405, #6735, #9179 ) ;
#3349 = DIRECTION ( 'NONE',  ( 0.000000000000000000, 1.000000000000000000, 0.000000000000000000 ) ) ;
#3350 = CARTESIAN_POINT ( 'NONE',  ( -1.929652039733607660, -2.791718527286190188, -0.1763362329223841507 ) ) ;
#3351 = ORIENTED_EDGE ( 'NONE', *, *, #5580, .T. ) ;
#3352 = DIRECTION ( 'NONE',  ( -0.8011800915434522663, 0.5984233124757303290, 0.000000000000000000 ) ) ;
#3353 = DIRECTION ( 'NONE',  ( -0.8660254037844398178, 0.000000000000000000, 0.4999999999999979461 ) ) ;
#3354 = EDGE_LOOP ( 'NONE', ( #4633, #5849, #3718, #12963 ) ) ;
#3355 = ORIENTED_EDGE ( 'NONE', *, *, #2420, .T. ) ;
#3356 = VECTOR ( 'NONE', #10960, 39.37007874015748143 ) ;
#3357 = AXIS2_PLACEMENT_3D ( 'NONE', #4434, #820, #2073 ) ;
#3358 = ADVANCED_FACE ( 'NONE', ( #7264 ), #10866, .F. ) ;
#3359 = AXIS2_PLACEMENT_3D ( 'NONE', #14184, #13163, #170 ) ;
#3360 = AXIS2_PLACEMENT_3D ( 'NONE', #13398, #179, #7278 ) ;
#3361 = ORIENTED_EDGE ( 'NONE', *, *, #3691, .T. ) ;
#3362 = AXIS2_PLACEMENT_3D ( 'NONE', #8649, #13428, #2697 ) ;
#3363 = EDGE_CURVE ( 'NONE', #6293, #381, #9332, .T. ) ;
#3364 = PLANE ( 'NONE',  #14382 ) ;
#3365 = AXIS2_PLACEMENT_3D ( 'NONE', #13345, #6128, #5980 ) ;
#3366 = EDGE_CURVE ( 'NONE', #2230, #241, #7492, .T. ) ;
#3367 = FACE_OUTER_BOUND ( 'NONE', #10027, .T. ) ;
#3368 = DIRECTION ( 'NONE',  ( -1.000000000000000000, -8.673617379884013384E-15, 0.000000000000000000 ) ) ;
#3369 = DIRECTION ( 'NONE',  ( 0.000000000000000000, 1.000000000000000000, 0.000000000000000000 ) ) ;
#3370 = VECTOR ( 'NONE', #10814, 39.37007874015748143 ) ;
#3371 = DIRECTION ( 'NONE',  ( -1.000000000000000000, 0.000000000000000000, 1.669238443041289401E-16 ) ) ;
#3372 = VECTOR ( 'NONE', #5343, 39.37007874015748143 ) ;
#3373 = VECTOR ( 'NONE', #809, 39.37007874015748143 ) ;
#3374 = CARTESIAN_POINT ( 'NONE',  ( -1.187740243782785310, 0.3305209984255342848, -0.05905511811023626823 ) ) ;
#3375 = CLOSED_SHELL ( 'NONE', ( #6514, #1739, #8747, #10679, #4028, #10850, #12204, #2441, #3423, #3390, #15096, #13546, #7794, #5987, #3039, #2984, #4995, #13673, #13545, #9675, #14527, #4144, #3358, #1488, #7299, #1392, #8111, #13367, #9133, #15005, #1837, #13001, #13053, #13157, #5419, #13148, #15175, #9742, #5781, #4228, #5482, #2719, #6524, #9045, #13905, #3780, #15024, #10780, #648, #3274, #7253, #7707, #6249, #5961, #8524, #1656, #9735, #8074, #2510, #14799, #9881, #7593, #2329, #9906, #1556, #14978, #13759, #14242, #4185, #2914, #12920, #12511, #818, #2413, #4549, #12373, #12502, #23, #4681, #9700, #6263, #6791, #2061, #11809, #4544, #10479, #13742, #2553, #3131, #14296, #9409, #1204, #2054, #7761, #10063, #7636, #200, #3674, #14921, #4075, #13724, #6455, #6756, #6810, #75, #1323, #12287, #4555, #9738, #801, #1524, #460, #10206, #10208, #725, #1653, #7479, #6601, #1422, #11899, #3298, #8467, #5739, #3913, #4002, #11933, #9163, #9760, #6642, #5538, #8172, #120, #3523, #916, #10709, #9229, #4715, #8055, #9834, #13249, #9929, #6321, #15437, #4626, #14600, #13128, #589, #9988, #6145, #10703, #2929, #606, #6817, #14037, #3973, #8816, #12806, #14014, #13828, #2894, #10225, #10258, #4529, #14216, #13840, #3835, #4426, #12557, #7876, #12052, #6951, #4961, #2081, #2217, #12840, #5894, #13963, #8558, #11327, #442, #11144, #5107, #12418, #11044, #6430, #4738, #1824, #11020, #8664, #15071, #10543, #8825, #5716, #10107, #12893, #3853, #13261, #9719, #9555, #3954, #13055, #11251, #6844, #5388, #8088, #3694, #5176, #2481, #14970, #13281, #12499, #585, #7969, #10894, #4528, #9301, #7572, #2327, #14505, #11682, #11052, #7304, #873, #11629, #8568, #7629, #929, #5198, #324, #11760, #6905, #2997, #11775, #9885 ) ) ;
#3376 = ORIENTED_EDGE ( 'NONE', *, *, #14019, .F. ) ;
#3377 = DIRECTION ( 'NONE',  ( -0.8660254037844365982, 0.000000000000000000, -0.5000000000000035527 ) ) ;
#3378 = DIRECTION ( 'NONE',  ( 0.000000000000000000, 1.000000000000000000, 2.224004456380530778E-16 ) ) ;
#3379 = AXIS2_PLACEMENT_3D ( 'NONE', #191, #14751, #5080 ) ;
#3380 = DIRECTION ( 'NONE',  ( 0.000000000000000000, 0.000000000000000000, -1.000000000000000000 ) ) ;
#3381 = FACE_OUTER_BOUND ( 'NONE', #5663, .T. ) ;
#3382 = ORIENTED_EDGE ( 'NONE', *, *, #1068, .T. ) ;
#3383 = FACE_OUTER_BOUND ( 'NONE', #8553, .T. ) ;
#3384 = ORIENTED_EDGE ( 'NONE', *, *, #10498, .T. ) ;
#3385 = ORIENTED_EDGE ( 'NONE', *, *, #6002, .F. ) ;
#3386 = EDGE_CURVE ( 'NONE', #6985, #4753, #6227, .T. ) ;
#3388 = ORIENTED_EDGE ( 'NONE', *, *, #3429, .F. ) ;
#3387 = AXIS2_PLACEMENT_3D ( 'NONE', #5543, #15209, #14026 ) ;
#3389 = CIRCLE ( 'NONE', #8638, 0.04330708661417331101 ) ;
#3390 = ADVANCED_FACE ( 'NONE', ( #13374 ), #12087, .T. ) ;
#3391 = EDGE_LOOP ( 'NONE', ( #8662, #12658, #13247, #11053 ) ) ;
#3392 = CIRCLE ( 'NONE', #5369, 0.007874015748031516770 ) ;
#3393 = SPHERICAL_SURFACE ( 'NONE', #8830, 0.003937007874015747977 ) ;
#3394 = DIRECTION ( 'NONE',  ( 0.000000000000000000, 0.000000000000000000, -1.000000000000000000 ) ) ;
#3395 = AXIS2_PLACEMENT_3D ( 'NONE', #935, #4596, #6957 ) ;
#3396 = EDGE_CURVE ( 'NONE', #14687, #12371, #6323, .T. ) ;
#3397 = DIRECTION ( 'NONE',  ( -1.000000000000000000, 0.000000000000000000, 0.000000000000000000 ) ) ;
#3398 = FACE_BOUND ( 'NONE', #11761, .T. ) ;
#3399 = CYLINDRICAL_SURFACE ( 'NONE', #10936, 0.01968503937007875723 ) ;
#3400 = CARTESIAN_POINT ( 'NONE',  ( -0.07635964791965738074, -0.1878198040935885327, 0.03937007874015747977 ) ) ;
#3401 = ORIENTED_EDGE ( 'NONE', *, *, #8404, .F. ) ;
#3402 = DIRECTION ( 'NONE',  ( 0.000000000000000000, -1.000000000000000000, 2.212657494868377674E-16 ) ) ;
#3403 = CARTESIAN_POINT ( 'NONE',  ( 0.000000000000000000, 0.05905511811023622659, 0.000000000000000000 ) ) ;
#3404 = CIRCLE ( 'NONE', #5381, 0.007874015748031482076 ) ;
#3405 = AXIS2_PLACEMENT_3D ( 'NONE', #9310, #1086, #2489 ) ;
#3406 = DIRECTION ( 'NONE',  ( 1.224646799147353947E-16, 0.000000000000000000, -1.000000000000000000 ) ) ;
#3407 = AXIS2_PLACEMENT_3D ( 'NONE', #11848, #1043, #9337 ) ;
#3408 = ORIENTED_EDGE ( 'NONE', *, *, #4324, .T. ) ;
#3409 = AXIS2_PLACEMENT_3D ( 'NONE', #12897, #12978, #2242 ) ;
#3410 = EDGE_LOOP ( 'NONE', ( #5694, #11551 ) ) ;
#3411 = DIRECTION ( 'NONE',  ( 0.5000000000000037748, -0.000000000000000000, 0.8660254037844365982 ) ) ;
#3412 = ORIENTED_EDGE ( 'NONE', *, *, #271, .T. ) ;
#3413 = EDGE_CURVE ( 'NONE', #6757, #3049, #13521, .T. ) ;
#3414 = EDGE_LOOP ( 'NONE', ( #10710, #9050, #12845, #13404 ) ) ;
#3415 = ORIENTED_EDGE ( 'NONE', *, *, #1306, .F. ) ;
#3416 = AXIS2_PLACEMENT_3D ( 'NONE', #11466, #737, #9104 ) ;
#3417 = DIRECTION ( 'NONE',  ( 0.8660254037844347108, 0.000000000000000000, 0.5000000000000069944 ) ) ;
#3418 = AXIS2_PLACEMENT_3D ( 'NONE', #4041, #8679, #298 ) ;
#3419 = B_SPLINE_CURVE_WITH_KNOTS ( 'NONE', 3,
 ( #12706, #5476, #10264, #641 ),
 .UNSPECIFIED., .F., .F.,
 ( 4, 4 ),
 ( 0.000000000000000000, 2.119993237936282563E-05 ),
 .UNSPECIFIED. ) ;
#3420 = EDGE_CURVE ( 'NONE', #4234, #2668, #92, .T. ) ;
#3421 = LINE ( 'NONE', #12891, #14350 ) ;
#3422 = DIRECTION ( 'NONE',  ( -0.8660254037844390407, 0.000000000000000000, 0.4999999999999994449 ) ) ;
#3423 = ADVANCED_FACE ( 'NONE', ( #1540 ), #13579, .T. ) ;
#3424 = DIRECTION ( 'NONE',  ( 0.5692328345973325376, 0.000000000000000000, -0.8221763679505059708 ) ) ;
#3425 = AXIS2_PLACEMENT_3D ( 'NONE', #2053, #9199, #3402 ) ;
#3426 = PRODUCT_DEFINITION_SHAPE ( 'NONE', 'NONE',  #15487 ) ;
#3427 = CARTESIAN_POINT ( 'NONE',  ( 0.4749369078591172411, -0.4881889763779528324, 0.3514880584999470203 ) ) ;
#3428 = DIRECTION ( 'NONE',  ( -1.000000000000000000, 0.000000000000000000, 0.000000000000000000 ) ) ;
#3429 = EDGE_CURVE ( 'NONE', #3736, #12889, #828, .T. ) ;
#3430 = CARTESIAN_POINT ( 'NONE',  ( -0.1618514667033796040, -0.1023622047244094474, 0.2161887458866224576 ) ) ;
#3431 = EDGE_CURVE ( 'NONE', #10081, #9980, #10664, .T. ) ;
#3432 = CARTESIAN_POINT ( 'NONE',  ( -1.491640810881974977, 0.2222636556240916994, -0.03937007874015747977 ) ) ;
#3433 = ORIENTED_EDGE ( 'NONE', *, *, #10545, .F. ) ;
#3434 = ORIENTED_EDGE ( 'NONE', *, *, #13330, .F. ) ;
#3435 = ORIENTED_EDGE ( 'NONE', *, *, #7014, .F. ) ;
#3436 = AXIS2_PLACEMENT_3D ( 'NONE', #9023, #13794, #6565 ) ;
#3437 = ORIENTED_EDGE ( 'NONE', *, *, #3269, .T. ) ;
#3438 = DIRECTION ( 'NONE',  ( 0.5000000000000051070, 0.000000000000000000, -0.8660254037844358210 ) ) ;
#3439 = AXIS2_PLACEMENT_3D ( 'NONE', #3232, #11602, #14109 ) ;
#3440 = CARTESIAN_POINT ( 'NONE',  ( -0.07874015748031489015, 0.1442356988431297560, 0.05905511811023622659 ) ) ;
#3441 = CARTESIAN_POINT ( 'NONE',  ( -0.5412723129863770133, 1.340161119985692428, 0.2430722610364171865 ) ) ;
#3442 = DIRECTION ( 'NONE',  ( 0.000000000000000000, 0.000000000000000000, 1.000000000000000000 ) ) ;
#3443 = VECTOR ( 'NONE', #11754, 39.37007874015748143 ) ;
#3444 = DIRECTION ( 'NONE',  ( 1.000000000000000000, 0.000000000000000000, 0.000000000000000000 ) ) ;
#3445 = ORIENTED_EDGE ( 'NONE', *, *, #4650, .F. ) ;
#3446 = DIRECTION ( 'NONE',  ( 0.000000000000000000, 0.000000000000000000, 1.000000000000000000 ) ) ;
#3447 = EDGE_CURVE ( 'NONE', #15003, #9212, #12132, .T. ) ;
#3448 = DIRECTION ( 'NONE',  ( 0.000000000000000000, -1.000000000000000000, 0.000000000000000000 ) ) ;
#3449 = ORIENTED_EDGE ( 'NONE', *, *, #6925, .F. ) ;
#3450 = ORIENTED_EDGE ( 'NONE', *, *, #3245, .F. ) ;
#3451 = VERTEX_POINT ( 'NONE', #6157 ) ;
#3452 = CYLINDRICAL_SURFACE ( 'NONE', #4116, 0.003937007874015758385 ) ;
#3453 = CARTESIAN_POINT ( 'NONE',  ( -0.1213717603336464113, 2.440944881889763884, -0.04263160285333146560 ) ) ;
#3454 = DIRECTION ( 'NONE',  ( -0.000000000000000000, -1.000000000000000000, -0.000000000000000000 ) ) ;
#3455 = DIRECTION ( 'NONE',  ( 0.5000000000000004441, 0.000000000000000000, 0.8660254037844383745 ) ) ;
#3457 = AXIS2_PLACEMENT_3D ( 'NONE', #6936, #12895, #2517 ) ;
#3456 = CARTESIAN_POINT ( 'NONE',  ( -1.220472440944881720, 0.000000000000000000, 0.02952755905511811330 ) ) ;
#3458 = CARTESIAN_POINT ( 'NONE',  ( -1.956732843150922774, -2.774109272326283460, 0.1775768436135731765 ) ) ;
#3459 = ORIENTED_EDGE ( 'NONE', *, *, #8930, .F. ) ;
#3460 = CYLINDRICAL_SURFACE ( 'NONE', #15439, 0.03937007874015751446 ) ;
#3461 = DIRECTION ( 'NONE',  ( -0.5000000000000001110, -0.000000000000000000, -0.8660254037844385966 ) ) ;
#3462 = CIRCLE ( 'NONE', #2707, 0.003937007874015749712 ) ;
#3463 = CARTESIAN_POINT ( 'NONE',  ( -0.5398975377803494347, -0.4881889763779528324, 0.2389729469846940679 ) ) ;
#3464 = DIRECTION ( 'NONE',  ( -1.504632769052536979E-28, 8.673617379884035472E-15, 1.000000000000000000 ) ) ;
#3465 = EDGE_LOOP ( 'NONE', ( #8824, #2807, #10507, #14291, #6716, #5433 ) ) ;
#3466 = DIRECTION ( 'NONE',  ( 0.000000000000000000, 0.000000000000000000, 1.000000000000000000 ) ) ;
#3467 = ORIENTED_EDGE ( 'NONE', *, *, #11307, .F. ) ;
#3468 = ADVANCED_FACE ( 'NONE', ( #10946 ), #7822, .T. ) ;
#3469 = ORIENTED_EDGE ( 'NONE', *, *, #8586, .F. ) ;
#3470 = ADVANCED_BREP_SHAPE_REPRESENTATION ( '', ( #9543, #11481 ), #7714 ) ;
#3471 = DIMENSIONAL_EXPONENTS ( 1.000000000000000000, 0.000000000000000000, 0.000000000000000000, 0.000000000000000000, 0.000000000000000000, 0.000000000000000000, 0.000000000000000000 ) ;
#3472 = ORIENTED_EDGE ( 'NONE', *, *, #12982, .T. ) ;
#3473 = AXIS2_PLACEMENT_3D ( 'NONE', #4071, #12310, #3930 ) ;
#3474 = DIRECTION ( 'NONE',  ( -0.000000000000000000, -1.000000000000000000, -0.000000000000000000 ) ) ;
#3475 = FACE_OUTER_BOUND ( 'NONE', #13018, .T. ) ;
#3476 = CARTESIAN_POINT ( 'NONE',  ( -1.606329852969329952, 0.09914256429936342541, -0.06530908795646298004 ) ) ;
#3477 = DIRECTION ( 'NONE',  ( 0.000000000000000000, 0.000000000000000000, 1.000000000000000000 ) ) ;
#3478 = CARTESIAN_POINT ( 'NONE',  ( -1.100415514366370306, -0.04998955061625946078, 0.03937007874015747977 ) ) ;
#3479 = CARTESIAN_POINT ( 'NONE',  ( -1.181846041278642456, 0.3414510595302567286, 0.04963318180378523820 ) ) ;
#3480 = ORIENTED_EDGE ( 'NONE', *, *, #10260, .T. ) ;
#3481 = EDGE_CURVE ( 'NONE', #7462, #12817, #5566, .T. ) ;
#3482 = DIRECTION ( 'NONE',  ( 0.5293839892290401750, -0.8483823383050519418, 0.000000000000000000 ) ) ;
#3483 = CARTESIAN_POINT ( 'NONE',  ( 0.5418660417173575272, -0.4881889763779528324, 0.2355633981508975516 ) ) ;
#3484 = CARTESIAN_POINT ( 'NONE',  ( -1.577626109319266945, 0.1055621384246793470, 0.06600777036542521126 ) ) ;
#3485 = DIRECTION ( 'NONE',  ( 0.4999999999999919509, -0.000000000000000000, -0.8660254037844432595 ) ) ;
#3486 = ADVANCED_FACE ( 'NONE', ( #1775, #7795 ), #6698, .F. ) ;
#3487 = DIRECTION ( 'NONE',  ( 1.224646799147353207E-16, 1.000000000000000000, 0.000000000000000000 ) ) ;
#3488 = EDGE_LOOP ( 'NONE', ( #13506, #7460, #8521, #13032 ) ) ;
#3489 = EDGE_CURVE ( 'NONE', #4456, #11475, #4122, .T. ) ;
#3490 = CYLINDRICAL_SURFACE ( 'NONE', #7183, 0.03937007874015759773 ) ;
#3491 = VERTEX_POINT ( 'NONE', #11411 ) ;
#3492 = ORIENTED_EDGE ( 'NONE', *, *, #1785, .F. ) ;
#3493 = EDGE_LOOP ( 'NONE', ( #8230, #14225, #4400, #11566 ) ) ;
#3494 = CARTESIAN_POINT ( 'NONE',  ( 0.000000000000000000, 1.377952755905512028, 0.000000000000000000 ) ) ;
#3495 = CARTESIAN_POINT ( 'NONE',  ( -0.05958257715034473434, -0.1023622047244094474, -0.2346892519263902022 ) ) ;
#3496 = CARTESIAN_POINT ( 'NONE',  ( -1.914045371080042246, -2.904349441506412610, -0.1187067027335292763 ) ) ;
#3497 =( LENGTH_UNIT ( ) NAMED_UNIT ( * ) SI_UNIT ( $, .METRE. ) );
#3498 = DIRECTION ( 'NONE',  ( -0.000000000000000000, 1.000000000000000000, 0.000000000000000000 ) ) ;
#3499 = CARTESIAN_POINT ( 'NONE',  ( 1.976792077363838002E-17, 0.003937007874015860734, 0.1614173228346456879 ) ) ;
#3500 = DIRECTION ( 'NONE',  ( 0.000000000000000000, 0.000000000000000000, -1.000000000000000000 ) ) ;
#3501 = ADVANCED_FACE ( 'NONE', ( #7649 ), #13765, .T. ) ;
#3502 = FACE_OUTER_BOUND ( 'NONE', #9550, .T. ) ;
#3503 = CARTESIAN_POINT ( 'NONE',  ( -0.4572203724260467950, -0.1023622047244094474, 0.3821739980041202744 ) ) ;
#3504 = ORIENTED_EDGE ( 'NONE', *, *, #11371, .T. ) ;
#3505 = EDGE_CURVE ( 'NONE', #8683, #288, #12587, .T. ) ;
#3506 = VERTEX_POINT ( 'NONE', #3104 ) ;
#3507 = EDGE_LOOP ( 'NONE', ( #13396, #3903, #2998, #10477, #5703 ) ) ;
#3508 = ORIENTED_EDGE ( 'NONE', *, *, #4452, .T. ) ;
#3509 = B_SPLINE_CURVE_WITH_KNOTS ( 'NONE', 3,
 ( #10781, #2406, #11982, #13361, #1307, #1242, #12205, #11008, #289, #14542 ),
 .UNSPECIFIED., .F., .F.,
 ( 4, 2, 2, 2, 4 ),
 ( 0.000000000000000000, 0.003638376726563020275, 0.007276753453126040549, 0.01455350690625210018, 0.02910701381250420036 ),
 .UNSPECIFIED. ) ;
#3510 = APPLICATION_CONTEXT ( 'automotive_design' ) ;
#3511 = CARTESIAN_POINT ( 'NONE',  ( -1.588298999900090935, 0.1240273096573925177, -0.05983744915167243938 ) ) ;
#3512 = CYLINDRICAL_SURFACE ( 'NONE', #12449, 0.03937007874015751446 ) ;
#3513 = DIRECTION ( 'NONE',  ( 0.000000000000000000, 0.000000000000000000, 1.000000000000000000 ) ) ;
#3514 = FACE_OUTER_BOUND ( 'NONE', #5717, .T. ) ;
#3515 = DIRECTION ( 'NONE',  ( -0.000000000000000000, -1.000000000000000000, -0.000000000000000000 ) ) ;
#3516 = ORIENTED_EDGE ( 'NONE', *, *, #6456, .F. ) ;
#3517 = LINE ( 'NONE', #3583, #198 ) ;
#3518 = DIRECTION ( 'NONE',  ( 1.000000000000000000, -0.000000000000000000, -0.000000000000000000 ) ) ;
#3519 = ORIENTED_EDGE ( 'NONE', *, *, #14792, .T. ) ;
#3520 = EDGE_LOOP ( 'NONE', ( #10805, #9206, #76, #9471 ) ) ;
#3521 = EDGE_CURVE ( 'NONE', #13356, #7138, #10304, .T. ) ;
#3522 = ORIENTED_EDGE ( 'NONE', *, *, #1889, .F. ) ;
#3523 = ADVANCED_FACE ( 'NONE', ( #6467 ), #527, .F. ) ;
#3524 = EDGE_CURVE ( 'NONE', #6704, #6873, #6148, .T. ) ;
#3525 = CARTESIAN_POINT ( 'NONE',  ( -1.938308666834797522, -2.949171973686980586, 0.01241952892555889601 ) ) ;
#3526 = CARTESIAN_POINT ( 'NONE',  ( -1.172017912842092446, 0.3609012623030118383, -0.03937007874015747977 ) ) ;
#3527 = CARTESIAN_POINT ( 'NONE',  ( 0.000000000000000000, 0.5590551181102362266, 0.5590551181102362266 ) ) ;
#3528 = DIRECTION ( 'NONE',  ( 3.476578583725179813E-16, 0.000000000000000000, -1.000000000000000000 ) ) ;
#3529 = CARTESIAN_POINT ( 'NONE',  ( -1.937743059600893769, -2.834246032412025329, 0.1664475769057940369 ) ) ;
#3530 = EDGE_LOOP ( 'NONE', ( #2806, #12968 ) ) ;
#3531 = DIRECTION ( 'NONE',  ( 0.8660254037844368202, 0.000000000000000000, -0.5000000000000032196 ) ) ;
#3532 = FACE_OUTER_BOUND ( 'NONE', #10549, .T. ) ;
#3533 = CARTESIAN_POINT ( 'NONE',  ( -0.04509495097506252548, 0.1479884890110656215, 0.05203401519686124549 ) ) ;
#3534 = CARTESIAN_POINT ( 'NONE',  ( -1.605558588137308451, 0.1002381878602953691, 0.06208189601213050246 ) ) ;
#3535 = ORIENTED_EDGE ( 'NONE', *, *, #4986, .T. ) ;
#3536 = VERTEX_POINT ( 'NONE', #12670 ) ;
#3537 = ORIENTED_EDGE ( 'NONE', *, *, #14769, .T. ) ;
#3538 = DIRECTION ( 'NONE',  ( -8.673617379884087537E-15, 0.000000000000000000, -1.000000000000000000 ) ) ;
#3539 = PRODUCT_DEFINITION ( 'UNKNOWN', '', #10378, #7819 ) ;
#3540 = CARTESIAN_POINT ( 'NONE',  ( 0.5860051159906327634, -0.003937007874015747977, 0.1591122789105293700 ) ) ;
#3541 = CARTESIAN_POINT ( 'NONE',  ( -1.394656322662437775, -0.02432159694977429829, 0.06446741476485348676 ) ) ;
#3542 = CARTESIAN_POINT ( 'NONE',  ( -0.07635964791965738074, -0.1878198040935885327, 0.03937007874015747977 ) ) ;
#3543 = DIRECTION ( 'NONE',  ( -1.000000000000000000, -0.000000000000000000, -0.000000000000000000 ) ) ;
#3544 = CYLINDRICAL_SURFACE ( 'NONE', #3874, 0.03937007874015751446 ) ;
#3545 = ORIENTED_EDGE ( 'NONE', *, *, #5318, .T. ) ;
#3546 = CARTESIAN_POINT ( 'NONE',  ( 0.1724006475077543565, -0.1023622047244094474, 0.1768186671464649640 ) ) ;
#3547 = DIRECTION ( 'NONE',  ( 1.000000000000000000, -0.000000000000000000, 1.224646799147353207E-16 ) ) ;
#3548 = CARTESIAN_POINT ( 'NONE',  ( -0.02018259705034725071, -0.1802452534892125813, 1.049219007154695292E-17 ) ) ;
#3549 = ORIENTED_EDGE ( 'NONE', *, *, #12608, .T. ) ;
#3550 = ORIENTED_EDGE ( 'NONE', *, *, #2745, .F. ) ;
#3551 = ORIENTED_EDGE ( 'NONE', *, *, #4251, .T. ) ;
#3552 = VERTEX_POINT ( 'NONE', #10071 ) ;
#3553 = ADVANCED_FACE ( 'NONE', ( #7554 ), #8833, .F. ) ;
#3554 = ORIENTED_EDGE ( 'NONE', *, *, #1986, .F. ) ;
#3555 = EDGE_CURVE ( 'NONE', #675, #9261, #11492, .T. ) ;
#3556 = CARTESIAN_POINT ( 'NONE',  ( -0.3441669734936866343, 2.010494531933507467, -0.05905511811023622659 ) ) ;
#3557 = CARTESIAN_POINT ( 'NONE',  ( -1.181102362204724310, 0.000000000000000000, 0.02952755905511811330 ) ) ;
#3558 = CARTESIAN_POINT ( 'NONE',  ( -0.1771653543307349921, 37.37889961492984270, -0.8267716535433081715 ) ) ;
#3559 = PRESENTATION_STYLE_ASSIGNMENT (( #5907 ) ) ;
#3560 = FACE_OUTER_BOUND ( 'NONE', #13634, .T. ) ;
#3561 = EDGE_CURVE ( 'NONE', #12057, #2746, #15021, .T. ) ;
#3562 = CARTESIAN_POINT ( 'NONE',  ( 0.000000000000000000, 0.07874015748031495954, -0.05298991407461853265 ) ) ;
#3563 = SPHERICAL_SURFACE ( 'NONE', #10872, 0.003937007874015747977 ) ;
#3564 = CARTESIAN_POINT ( 'NONE',  ( -1.414416440118313689, -0.03985156058301880105, 0.05915390547199540078 ) ) ;
#3565 = CARTESIAN_POINT ( 'NONE',  ( -0.2762316197870718359, -0.2952755905511811330, 0.2731340278359842277 ) ) ;
#3566 = ORIENTED_EDGE ( 'NONE', *, *, #14500, .T. ) ;
#3567 = ORIENTED_EDGE ( 'NONE', *, *, #9619, .T. ) ;
#3568 = ORIENTED_EDGE ( 'NONE', *, *, #9306, .T. ) ;
#3569 = EDGE_LOOP ( 'NONE', ( #8308, #8704, #8962, #7352, #6449, #4058, #8937, #5159, #11416, #4259 ) ) ;
#3570 = EDGE_CURVE ( 'NONE', #6704, #8323, #9589, .T. ) ;
#3571 = EDGE_CURVE ( 'NONE', #856, #14746, #8771, .T. ) ;
#3572 = FACE_BOUND ( 'NONE', #6977, .T. ) ;
#3573 = CARTESIAN_POINT ( 'NONE',  ( -0.03967601873943667895, 0.1701129415451466120, 0.04931034005879585819 ) ) ;
#3574 = B_SPLINE_CURVE_WITH_KNOTS ( 'NONE', 3,
 ( #11047, #14582, #331, #8717, #5169 ),
 .UNSPECIFIED., .F., .F.,
 ( 4, 1, 4 ),
 ( 2.212246760591329979E-07, 0.001154921763055310937, 0.002309622301434562965 ),
 .UNSPECIFIED. ) ;
#3575 = ADVANCED_FACE ( 'NONE', ( #9058 ), #1625, .F. ) ;
#3576 = CARTESIAN_POINT ( 'NONE',  ( -0.05905511811012585655, -0.09842519685039370636, -0.5870514566507987197 ) ) ;
#3577 = EDGE_CURVE ( 'NONE', #10762, #14238, #13622, .T. ) ;
#3578 = CARTESIAN_POINT ( 'NONE',  ( -0.2344791876353258253, -0.1023622047244094474, 0.06718564542474284029 ) ) ;
#3579 = TOROIDAL_SURFACE ( 'NONE', #10086, 0.5984251968503937480, 0.007874015748031495954 ) ;
#3580 = CIRCLE ( 'NONE', #12335, 0.003937007874015758385 ) ;
#3581 = FACE_OUTER_BOUND ( 'NONE', #4290, .T. ) ;
#3582 = ORIENTED_EDGE ( 'NONE', *, *, #7503, .T. ) ;
#3583 = CARTESIAN_POINT ( 'NONE',  ( 0.1552072824047652233, -0.09842519685039370636, -0.5909884645248143498 ) ) ;
#3584 = AXIS2_PLACEMENT_3D ( 'NONE', #10161, #12516, #5277 ) ;
#3585 = DIRECTION ( 'NONE',  ( 1.000000000000000000, 0.000000000000000000, -1.224646799147353207E-16 ) ) ;
#3586 = DIRECTION ( 'NONE',  ( -0.000000000000000000, -0.000000000000000000, -1.000000000000000000 ) ) ;
#3587 = TOROIDAL_SURFACE ( 'NONE', #2824, 0.04330708661417328326, 0.003937007874015747977 ) ;
#3588 = ORIENTED_EDGE ( 'NONE', *, *, #12047, .F. ) ;
#3589 =( BOUNDED_SURFACE ( )  B_SPLINE_SURFACE ( 3, 2, ( 
 ( #4770, #9556, #14327 ),
 ( #3597, #6009, #8375 ),
 ( #9640, #8459, #14418 ),
 ( #2495, #7270, #10878 ),
 ( #167, #4052, #3989 ),
 ( #13609, #4134, #12594 ) ),
 .UNSPECIFIED., .F., .F., .T. ) 
 B_SPLINE_SURFACE_WITH_KNOTS ( ( 4, 2, 4 ),
 ( 3, 3 ),
 ( 0.003230360849850193086, 0.003748134328102737875, 0.004265907806355283098 ),
 ( 0.000000000000000000, 1.000000000000000000 ),
 .UNSPECIFIED. ) 
 GEOMETRIC_REPRESENTATION_ITEM ( )  RATIONAL_B_SPLINE_SURFACE ( (
 ( 1.000000000000000000, 0.7048936089935846638, 1.000000000000000000),
 ( 1.000000000000000000, 0.7048811933886807157, 1.000000000000000000),
 ( 1.000000000000000000, 0.7052257929052021534, 1.000000000000000000),
 ( 1.000000000000000000, 0.7061645128347127098, 1.000000000000000000),
 ( 1.000000000000000000, 0.7067576505881709714, 1.000000000000000000),
 ( 1.000000000000000000, 0.7070941911968886551, 1.000000000000000000) ) ) 
 REPRESENTATION_ITEM ( '' )  SURFACE ( )  );
#3590 = ORIENTED_EDGE ( 'NONE', *, *, #12364, .T. ) ;
#3591 = ORIENTED_EDGE ( 'NONE', *, *, #5413, .T. ) ;
#3592 = AXIS2_PLACEMENT_3D ( 'NONE', #1168, #5039, #9840 ) ;
#3593 = AXIS2_PLACEMENT_3D ( 'NONE', #10699, #8422, #13207 ) ;
#3594 = CARTESIAN_POINT ( 'NONE',  ( -0.1574803149606299191, -1.743072535964414816E-17, 0.000000000000000000 ) ) ;
#3595 = CIRCLE ( 'NONE', #14599, 0.003937007874015750579 ) ;
#3596 = AXIS2_PLACEMENT_3D ( 'NONE', #13349, #1596, #511 ) ;
#3597 = CARTESIAN_POINT ( 'NONE',  ( -1.580080891959756428, 0.1020406297964638193, 0.07533316186188826480 ) ) ;
#3598 = CARTESIAN_POINT ( 'NONE',  ( -1.942764639580312203, -2.938468699076707491, -0.06187511347702391584 ) ) ;
#3599 = CARTESIAN_POINT ( 'NONE',  ( 0.4478092776764652783, 1.043307086614173373, 0.3267337836880532809 ) ) ;
#3600 = EDGE_CURVE ( 'NONE', #713, #12819, #2080, .T. ) ;
#3601 = DIRECTION ( 'NONE',  ( 1.000000000000000000, 0.000000000000000000, -1.224646799147353207E-16 ) ) ;
#3602 = ADVANCED_FACE ( 'NONE', ( #3502 ), #8575, .F. ) ;
#3603 = DIRECTION ( 'NONE',  ( -1.000000000000000000, 0.000000000000000000, 0.000000000000000000 ) ) ;
#3604 = CARTESIAN_POINT ( 'NONE',  ( -1.945459748359985808, -2.745801194614590823, 0.1561691687464104583 ) ) ;
#3605 = EDGE_LOOP ( 'NONE', ( #6924, #14272, #14919 ) ) ;
#3606 = CARTESIAN_POINT ( 'NONE',  ( -1.995626487841946295, -2.802056568083358012, -0.1561605048222872716 ) ) ;
#3607 = FACE_OUTER_BOUND ( 'NONE', #73, .T. ) ;
#3608 = CIRCLE ( 'NONE', #6832, 0.007874015748031516770 ) ;
#3609 = AXIS2_PLACEMENT_3D ( 'NONE', #1518, #4019, #11059 ) ;
#3610 = DIRECTION ( 'NONE',  ( 0.000000000000000000, -0.000000000000000000, -1.000000000000000000 ) ) ;
#3611 = EDGE_LOOP ( 'NONE', ( #6278, #7784, #3639, #15302 ) ) ;
#3612 = AXIS2_PLACEMENT_3D ( 'NONE', #13484, #1733, #6492 ) ;
#3613 = ADVANCED_FACE ( 'NONE', ( #12983 ), #12838, .T. ) ;
#3614 = AXIS2_PLACEMENT_3D ( 'NONE', #10666, #13078, #2435 ) ;
#3615 = AXIS2_PLACEMENT_3D ( 'NONE', #6816, #9436, #15226 ) ;
#3616 = ORIENTED_EDGE ( 'NONE', *, *, #4138, .T. ) ;
#3617 = VERTEX_POINT ( 'NONE', #2245 ) ;
#3618 = CARTESIAN_POINT ( 'NONE',  ( -0.06692913385815728311, -0.2952755905511811330, -0.4190977005962941426 ) ) ;
#3619 = LINE ( 'NONE', #1121, #14597 ) ;
#3620 = CIRCLE ( 'NONE', #9124, 0.003937007874015750579 ) ;
#3621 = CIRCLE ( 'NONE', #10871, 0.1614173228346456879 ) ;
#3622 = AXIS2_PLACEMENT_3D ( 'NONE', #3873, #4808, #14698 ) ;
#3623 = CIRCLE ( 'NONE', #3359, 0.1476377952755905942 ) ;
#3624 = CARTESIAN_POINT ( 'NONE',  ( 6.750021727583836750E-17, 0.000000000000000000, 0.5511811023622046335 ) ) ;
#3625 = CONTEXT_DEPENDENT_SHAPE_REPRESENTATION ( #5391, #2794 ) ;
#3626 = FACE_OUTER_BOUND ( 'NONE', #1328, .T. ) ;
#3627 = AXIS2_PLACEMENT_3D ( 'NONE', #7450, #12246, #1503 ) ;
#3628 = CARTESIAN_POINT ( 'NONE',  ( 0.000000000000000000, 0.07874015748031495954, -0.03937007874015751446 ) ) ;
#3629 = DIRECTION ( 'NONE',  ( 0.000000000000000000, 0.000000000000000000, 1.000000000000000000 ) ) ;
#3630 = ORIENTED_EDGE ( 'NONE', *, *, #3035, .T. ) ;
#3631 = CARTESIAN_POINT ( 'NONE',  ( 0.05905511811023622659, 1.190944881889763884, -0.8267716535433072833 ) ) ;
#3632 = DIRECTION ( 'NONE',  ( 0.5000000000000036637, -0.000000000000000000, 0.8660254037844364872 ) ) ;
#3633 = CARTESIAN_POINT ( 'NONE',  ( -1.496171808639726875, 0.2144740403064263057, -0.05905511811023622659 ) ) ;
#3634 = EDGE_CURVE ( 'NONE', #6948, #5863, #12626, .T. ) ;
#3635 = CARTESIAN_POINT ( 'NONE',  ( -0.1743691514447623103, -0.1023622047244094474, 0.1734091183126679758 ) ) ;
#3636 = CIRCLE ( 'NONE', #4861, 0.003937007874015741038 ) ;
#3637 = CIRCLE ( 'NONE', #1631, 0.03937007874015751446 ) ;
#3638 = VECTOR ( 'NONE', #7427, 39.37007874015748854 ) ;
#3639 = ORIENTED_EDGE ( 'NONE', *, *, #409, .F. ) ;
#3640 = VERTEX_POINT ( 'NONE', #8207 ) ;
#3641 = EDGE_LOOP ( 'NONE', ( #8941, #11348, #1007, #6471 ) ) ;
#3642 = ORIENTED_EDGE ( 'NONE', *, *, #2199, .F. ) ;
#3643 = LINE ( 'NONE', #4798, #11920 ) ;
#3644 = CYLINDRICAL_SURFACE ( 'NONE', #6579, 0.003937007874015743640 ) ;
#3645 = CARTESIAN_POINT ( 'NONE',  ( -1.904703986270961824, -2.930671797127443412, 0.08032951875385678508 ) ) ;
#3646 = DIRECTION ( 'NONE',  ( 2.775557561562891351E-17, 0.8219459448134281976, -0.5695655044020492275 ) ) ;
#3647 = VECTOR ( 'NONE', #957, 39.37007874015748143 ) ;
#3648 = FACE_OUTER_BOUND ( 'NONE', #4107, .T. ) ;
#3649 = CIRCLE ( 'NONE', #3886, 0.03937007874015751446 ) ;
#3650 = DIRECTION ( 'NONE',  ( 0.4999999999999918954, -0.000000000000000000, -0.8660254037844431485 ) ) ;
#3651 = AXIS2_PLACEMENT_3D ( 'NONE', #13426, #3947, #1291 ) ;
#3652 = CARTESIAN_POINT ( 'NONE',  ( 1.181102362204724310, 4.044111181948214319E-16, 0.02559055118110236185 ) ) ;
#3653 = CARTESIAN_POINT ( 'NONE',  ( -1.181102362204724310, 0.000000000000000000, -0.02559055118110236185 ) ) ;
#3654 = CIRCLE ( 'NONE', #410, 0.003937007874015758385 ) ;
#3655 = CARTESIAN_POINT ( 'NONE',  ( -0.1724006475077544398, -0.1023622047244094474, 0.1689446513984334541 ) ) ;
#3656 = LINE ( 'NONE', #9693, #9683 ) ;
#3657 = EDGE_CURVE ( 'NONE', #10478, #10993, #1823, .T. ) ;
#3658 = EDGE_LOOP ( 'NONE', ( #2127, #3282, #1212, #3467 ) ) ;
#3659 = TOROIDAL_SURFACE ( 'NONE', #4140, 0.03937007874015747977, 0.01968503937007873988 ) ;
#3660 = ORIENTED_EDGE ( 'NONE', *, *, #11856, .T. ) ;
#3661=STYLED_ITEM('',(#15519),#9119);
#3662 = AXIS2_PLACEMENT_3D ( 'NONE', #11747, #6864, #10311 ) ;
#3663 = ORIENTED_EDGE ( 'NONE', *, *, #720, .F. ) ;
#3664 = EDGE_CURVE ( 'NONE', #3964, #9996, #7863, .T. ) ;
#3665 = CIRCLE ( 'NONE', #13167, 0.007874015748031449116 ) ;
#3666 = CARTESIAN_POINT ( 'NONE',  ( -0.1574803149606299191, 0.000000000000000000, -0.5870514566507987197 ) ) ;
#3667 = CARTESIAN_POINT ( 'NONE',  ( -0.06299212598414173636, -0.4921259842519685179, -0.2377126739438355507 ) ) ;
#3668 = DIRECTION ( 'NONE',  ( 0.5000000000000035527, 0.000000000000000000, -0.8660254037844365982 ) ) ;
#3669 = LINE ( 'NONE', #4759, #1405 ) ;
#3670 = CARTESIAN_POINT ( 'NONE',  ( -0.1062992125983150266, -0.1023622047244094474, -0.2482618547482104143 ) ) ;
#3671 = TOROIDAL_SURFACE ( 'NONE', #13921, 0.5433070866141731514, 0.007874015748031495954 ) ;
#3672 = CARTESIAN_POINT ( 'NONE',  ( 0.000000000000000000, 0.000000000000000000, -0.7086614173228346081 ) ) ;
#3673 = CARTESIAN_POINT ( 'NONE',  ( -1.607606114292111199, 0.09732815221480045631, 0.1968503937007874127 ) ) ;
#3674 = ADVANCED_FACE ( 'NONE', ( #1069 ), #2074, .T. ) ;
#3675 = AXIS2_PLACEMENT_3D ( 'NONE', #6422, #4235, #5168 ) ;
#3676 = ADVANCED_FACE ( 'NONE', ( #15173 ), #10076, .T. ) ;
#3677 = VERTEX_POINT ( 'NONE', #3260 ) ;
#3678 = VERTEX_POINT ( 'NONE', #11648 ) ;
#3679 = EDGE_CURVE ( 'NONE', #10253, #12219, #8031, .T. ) ;
#3680 = ORIENTED_EDGE ( 'NONE', *, *, #12080, .F. ) ;
#3681 = AXIS2_PLACEMENT_3D ( 'NONE', #3940, #8720, #9579 ) ;
#3682 = FACE_OUTER_BOUND ( 'NONE', #3816, .T. ) ;
#3683 = VECTOR ( 'NONE', #15105, 39.37007874015747433 ) ;
#3684 = CARTESIAN_POINT ( 'NONE',  ( 0.4572203724260462399, -0.4881889763779528324, 0.3821739980041199969 ) ) ;
#3685 = DIRECTION ( 'NONE',  ( 0.000000000000000000, -1.000000000000000000, 2.222614453595283597E-16 ) ) ;
#3686 = CARTESIAN_POINT ( 'NONE',  ( 6.701807286672523049E-17, 0.03937007874015749365, 0.5433070866141731514 ) ) ;
#3687 = CARTESIAN_POINT ( 'NONE',  ( 0.000000000000000000, 2.448818897637795367, 0.04724409448818898266 ) ) ;
#3688 = CARTESIAN_POINT ( 'NONE',  ( -1.924909868815465996, -2.804990923292145499, 0.1525883533589904306 ) ) ;
#3689 = ORIENTED_EDGE ( 'NONE', *, *, #4242, .T. ) ;
#3690 = CARTESIAN_POINT ( 'NONE',  ( -1.945817195785428888, -2.931010914885669560, 0.04553526292943101822 ) ) ;
#3691 = EDGE_CURVE ( 'NONE', #7200, #1542, #6851, .T. ) ;
#3692 = VECTOR ( 'NONE', #1258, 39.37007874015748143 ) ;
#3693 = CARTESIAN_POINT ( 'NONE',  ( -0.03749734052841494775, 0.1488898142811246883, -0.04795046931071422075 ) ) ;
#3694 = ADVANCED_FACE ( 'NONE', ( #8115 ), #11740, .T. ) ;
#3695 = VERTEX_POINT ( 'NONE', #11560 ) ;
#3696 = ORIENTED_EDGE ( 'NONE', *, *, #12090, .T. ) ;
#3697 = EDGE_CURVE ( 'NONE', #3768, #9440, #8273, .T. ) ;
#3698 = EDGE_CURVE ( 'NONE', #8390, #6217, #10089, .T. ) ;
#3699 = AXIS2_PLACEMENT_3D ( 'NONE', #10195, #10034, #2909 ) ;
#3700 = VERTEX_POINT ( 'NONE', #10705 ) ;
#3701 = FACE_OUTER_BOUND ( 'NONE', #6675, .T. ) ;
#3702 = AXIS2_PLACEMENT_3D ( 'NONE', #9843, #3892, #368 ) ;
#3703 = EDGE_CURVE ( 'NONE', #7421, #4739, #2004, .T. ) ;
#3704 = CARTESIAN_POINT ( 'NONE',  ( -1.414149037809793619, -0.03961791295443582717, 0.05846194000333194973 ) ) ;
#3705 = DIRECTION ( 'NONE',  ( 0.000000000000000000, -1.000000000000000000, -0.000000000000000000 ) ) ;
#3706 = CIRCLE ( 'NONE', #13971, 0.003937007874015749712 ) ;
#3707 = CARTESIAN_POINT ( 'NONE',  ( 0.000000000000000000, 0.007874015748031480341, 0.000000000000000000 ) ) ;
#3708 = PLANE ( 'NONE',  #131 ) ;
#3709 = ORIENTED_EDGE ( 'NONE', *, *, #5266, .F. ) ;
#3710 = CARTESIAN_POINT ( 'NONE',  ( 0.4296613173079339432, -0.09448818897637796532, 0.4299076816772811060 ) ) ;
#3711 = DIRECTION ( 'NONE',  ( 0.000000000000000000, 0.000000000000000000, -1.000000000000000000 ) ) ;
#3712 = CARTESIAN_POINT ( 'NONE',  ( -0.04497577134311978031, -0.1837750859334940368, 0.03094209595079721806 ) ) ;
#3713 = CARTESIAN_POINT ( 'NONE',  ( 0.06692913385832208184, -0.2952755905511811330, -0.4190977005962941426 ) ) ;
#3714 = CIRCLE ( 'NONE', #13723, 0.01968503937007871213 ) ;
#3715 = ORIENTED_EDGE ( 'NONE', *, *, #2300, .T. ) ;
#3716 = ORIENTED_EDGE ( 'NONE', *, *, #6055, .F. ) ;
#3717 = EDGE_CURVE ( 'NONE', #13695, #4234, #5317, .T. ) ;
#3718 = ORIENTED_EDGE ( 'NONE', *, *, #7387, .T. ) ;
#3719 = AXIS2_PLACEMENT_3D ( 'NONE', #3890, #8671, #3806 ) ;
#3720 = ORIENTED_EDGE ( 'NONE', *, *, #5549, .T. ) ;
#3721 = CARTESIAN_POINT ( 'NONE',  ( -1.276200637803905691, -0.1988000726501942539, 0.05905511811023622659 ) ) ;
#3722 = EDGE_CURVE ( 'NONE', #14128, #5248, #9884, .T. ) ;
#3723 = EDGE_CURVE ( 'NONE', #10712, #925, #11567, .T. ) ;
#3724 = DIRECTION ( 'NONE',  ( 0.000000000000000000, 1.000000000000000000, 0.000000000000000000 ) ) ;
#3725 = CARTESIAN_POINT ( 'NONE',  ( 0.06299212598430634080, -0.4921259842519685179, -0.2377126739437405434 ) ) ;
#3726 = DIRECTION ( 'NONE',  ( 2.220446049250313081E-16, 0.8657846595920662969, -0.5004167495348750272 ) ) ;
#3727 = VECTOR ( 'NONE', #4843, 39.37007874015748143 ) ;
#3728 = DIRECTION ( 'NONE',  ( -0.000000000000000000, -1.000000000000000000, -0.000000000000000000 ) ) ;
#3729 = B_SPLINE_CURVE_WITH_KNOTS ( 'NONE', 3,
 ( #15364, #11837, #11771, #13015, #3534, #12939, #14106, #21, #1111, #2275 ),
 .UNSPECIFIED., .F., .F.,
 ( 4, 2, 2, 2, 4 ),
 ( 0.000000000000000000, 0.0002596010170527390326, 0.0005192020341054780653, 0.0007788030511582170979, 0.001038404068210956131 ),
 .UNSPECIFIED. ) ;
#3730 = CARTESIAN_POINT ( 'NONE',  ( -0.1724006475077544398, -0.09842519685039370636, 0.1768186671464649640 ) ) ;
#3731 = DIRECTION ( 'NONE',  ( -0.9900370584898828819, -0.1408070410764336311, -0.000000000000000000 ) ) ;
#3732 = FACE_BOUND ( 'NONE', #2772, .T. ) ;
#3733 = B_SPLINE_CURVE_WITH_KNOTS ( 'NONE', 3,
 ( #9197, #3310, #11785, #13976, #15228, #9116, #10520, #3400 ),
 .UNSPECIFIED., .F., .F.,
 ( 4, 2, 2, 4 ),
 ( 0.000000000000000000, 0.0009364989265740226044, 0.001404748389861033581, 0.001872997853148044775 ),
 .UNSPECIFIED. ) ;
#3734 = CYLINDRICAL_SURFACE ( 'NONE', #13098, 0.01968503937007875723 ) ;
#3735 = CARTESIAN_POINT ( 'NONE',  ( -0.5576140732134202693, -0.1023622047244094474, 0.2082870074805209804 ) ) ;
#3736 = VERTEX_POINT ( 'NONE', #9600 ) ;
#3737 = ORIENTED_EDGE ( 'NONE', *, *, #11173, .F. ) ;
#3738 = ORIENTED_EDGE ( 'NONE', *, *, #894, .F. ) ;
#3739 = DIRECTION ( 'NONE',  ( 0.000000000000000000, 0.000000000000000000, 1.000000000000000000 ) ) ;
#3740 = FACE_OUTER_BOUND ( 'NONE', #14665, .T. ) ;
#3741 = CARTESIAN_POINT ( 'NONE',  ( -1.181102362204724310, -0.1240157480314959815, -0.02952755905511811330 ) ) ;
#3742 = DIRECTION ( 'NONE',  ( 0.5000000000000001110, -0.000000000000000000, -0.8660254037844388186 ) ) ;
#3743 = CARTESIAN_POINT ( 'NONE',  ( 8.196454954923229282E-17, 1.425196850393700920, 0.6692913385826770867 ) ) ;
#3744 = DIRECTION ( 'NONE',  ( 1.000000000000000000, -0.000000000000000000, 0.000000000000000000 ) ) ;
#3745 = DIRECTION ( 'NONE',  ( 6.505213034913065258E-15, -1.000000000000000000, 0.000000000000000000 ) ) ;
#3746 = CYLINDRICAL_SURFACE ( 'NONE', #13833, 0.5905511811023621549 ) ;
#3747 = DIRECTION ( 'NONE',  ( 0.5000000000000004441, -0.000000000000000000, -0.8660254037844383745 ) ) ;
#3748 = ORIENTED_EDGE ( 'NONE', *, *, #3103, .T. ) ;
#3749 = ORIENTED_EDGE ( 'NONE', *, *, #6550, .T. ) ;
#3750 = ORIENTED_EDGE ( 'NONE', *, *, #14016, .T. ) ;
#3751 = EDGE_LOOP ( 'NONE', ( #5283, #11890, #7544, #7950 ) ) ;
#3752 = DIRECTION ( 'NONE',  ( 0.000000000000000000, 0.000000000000000000, -1.000000000000000000 ) ) ;
#3753 = EDGE_CURVE ( 'NONE', #2454, #2526, #9605, .T. ) ;
#3754 = DIRECTION ( 'NONE',  ( 1.000000000000000000, -0.000000000000000000, -0.000000000000000000 ) ) ;
#3755 = EDGE_CURVE ( 'NONE', #562, #14454, #9347, .T. ) ;
#3756 = CARTESIAN_POINT ( 'NONE',  ( -1.293236445124221312, 0.1355266887446167634, 0.05905511811023622659 ) ) ;
#3757 = DIRECTION ( 'NONE',  ( 0.9482728725910103407, 0.3174563893009453297, 0.000000000000000000 ) ) ;
#3758 = DIRECTION ( 'NONE',  ( -1.000000000000000000, 0.000000000000000000, 0.000000000000000000 ) ) ;
#3759 = DIRECTION ( 'NONE',  ( 0.000000000000000000, 1.000000000000000000, 0.000000000000000000 ) ) ;
#3760 = CARTESIAN_POINT ( 'NONE',  ( -1.931769569189934588, -2.785717222541405302, 0.1768902618314421582 ) ) ;
#3761 = ORIENTED_EDGE ( 'NONE', *, *, #6814, .F. ) ;
#3762 = CARTESIAN_POINT ( 'NONE',  ( -2.080881322745466999, -1.632190302820504479, -0.08366141732283423338 ) ) ;
#3763 = EDGE_CURVE ( 'NONE', #14414, #3640, #3595, .T. ) ;
#3764 = CARTESIAN_POINT ( 'NONE',  ( -1.570493619109850858, 0.1151020441255655169, 0.05905511811023620578 ) ) ;
#3765 = PLANE ( 'NONE',  #716 ) ;
#3766 = ORIENTED_EDGE ( 'NONE', *, *, #11912, .T. ) ;
#3767 = ORIENTED_EDGE ( 'NONE', *, *, #3489, .T. ) ;
#3768 = VERTEX_POINT ( 'NONE', #12399 ) ;
#3769 = EDGE_CURVE ( 'NONE', #10725, #11669, #13846, .T. ) ;
#3770 = CARTESIAN_POINT ( 'NONE',  ( -0.05114323250695503725, 0.05905511811023622659, -0.08858267716535432601 ) ) ;
#3771 = ADVANCED_FACE ( 'NONE', ( #2395 ), #6318, .T. ) ;
#3772 = CARTESIAN_POINT ( 'NONE',  ( 8.196454954923229282E-17, 0.000000000000000000, 0.6692913385826770867 ) ) ;
#3773 =( BOUNDED_CURVE ( )  B_SPLINE_CURVE ( 3, ( #9844, #13058, #2316, #7099 ),
 .UNSPECIFIED., .F., .T. ) 
 B_SPLINE_CURVE_WITH_KNOTS ( ( 4, 4 ),
 ( 1.040679608290689506, 1.570796326794894560 ),
 .UNSPECIFIED. ) 
 CURVE ( )  GEOMETRIC_REPRESENTATION_ITEM ( )  RATIONAL_B_SPLINE_CURVE ( ( 1.000000000000000000, 0.9767181429392493008, 0.9767181429392493008, 1.000000000000000000 ) ) 
 REPRESENTATION_ITEM ( '' )  );
#3774 = FACE_OUTER_BOUND ( 'NONE', #5509, .T. ) ;
#3775 = CYLINDRICAL_SURFACE ( 'NONE', #6679, 8.689140419947479543 ) ;
#3776 = LINE ( 'NONE', #2814, #12723 ) ;
#3777 = DIRECTION ( 'NONE',  ( -0.000000000000000000, -0.000000000000000000, -1.000000000000000000 ) ) ;
#3778 = EDGE_LOOP ( 'NONE', ( #10435, #11353, #831, #1252 ) ) ;
#3779 = LINE ( 'NONE', #33, #11156 ) ;
#3780 = ADVANCED_FACE ( 'NONE', ( #8429 ), #8504, .F. ) ;
#3781 = LINE ( 'NONE', #11216, #2593 ) ;
#3782 = CARTESIAN_POINT ( 'NONE',  ( -1.187897409289509376, 0.3305577418844916071, -0.05905511811023633761 ) ) ;
#3783 = DIRECTION ( 'NONE',  ( 0.5000000000000051070, 0.000000000000000000, -0.8660254037844358210 ) ) ;
#3784 =( NAMED_UNIT ( * ) PLANE_ANGLE_UNIT ( ) SI_UNIT ( $, .RADIAN. ) );
#3785 = ORIENTED_EDGE ( 'NONE', *, *, #4758, .F. ) ;
#3786 = EDGE_LOOP ( 'NONE', ( #13035, #2505, #11045, #2556 ) ) ;
#3787 = ORIENTED_EDGE ( 'NONE', *, *, #5519, .F. ) ;
#3788 = ORIENTED_EDGE ( 'NONE', *, *, #2278, .T. ) ;
#3789 = DIRECTION ( 'NONE',  ( 0.000000000000000000, 0.000000000000000000, -1.000000000000000000 ) ) ;
#3790 = DIRECTION ( 'NONE',  ( 0.000000000000000000, -0.000000000000000000, 1.000000000000000000 ) ) ;
#3791 = DIRECTION ( 'NONE',  ( 0.000000000000000000, 1.000000000000000000, 0.000000000000000000 ) ) ;
#3792 = DIRECTION ( 'NONE',  ( -0.4932581959314696340, 0.8219459448134285307, 0.2847827522010276668 ) ) ;
#3793 = LINE ( 'NONE', #8564, #2601 ) ;
#3794 = LINE ( 'NONE', #283, #1920 ) ;
#3795 = PLANE ( 'NONE',  #12116 ) ;
#3796 = EDGE_CURVE ( 'NONE', #2559, #2631, #5244, .T. ) ;
#3797 = FACE_OUTER_BOUND ( 'NONE', #10459, .T. ) ;
#3798 =( REPRESENTATION_RELATIONSHIP ('NONE','NONE', #8904, #2403 ) REPRESENTATION_RELATIONSHIP_WITH_TRANSFORMATION ( #8627 )SHAPE_REPRESENTATION_RELATIONSHIP( ) );
#3799 = DIRECTION ( 'NONE',  ( 0.000000000000000000, 0.000000000000000000, -1.000000000000000000 ) ) ;
#3800 = DIRECTION ( 'NONE',  ( -0.000000000000000000, -1.000000000000000000, -0.000000000000000000 ) ) ;
#3801 = ORIENTED_EDGE ( 'NONE', *, *, #15337, .F. ) ;
#3802 = EDGE_CURVE ( 'NONE', #12827, #796, #1623, .T. ) ;
#3803 = ORIENTED_EDGE ( 'NONE', *, *, #3413, .F. ) ;
#3804 = ORIENTED_EDGE ( 'NONE', *, *, #8820, .T. ) ;
#3805 = DIRECTION ( 'NONE',  ( -0.000000000000000000, 0.000000000000000000, 1.000000000000000000 ) ) ;
#3806 = DIRECTION ( 'NONE',  ( 0.000000000000000000, 0.000000000000000000, -1.000000000000000000 ) ) ;
#3807 = CARTESIAN_POINT ( 'NONE',  ( -1.431036756819010769, -0.02829858486107874466, -0.08366141732283458032 ) ) ;
#3808 = FACE_OUTER_BOUND ( 'NONE', #5213, .T. ) ;
#3809 = DIRECTION ( 'NONE',  ( 0.000000000000000000, 0.000000000000000000, 1.000000000000000000 ) ) ;
#3810 = CARTESIAN_POINT ( 'NONE',  ( 0.1531294576121448037, -0.4921259842519685179, -0.08840933357323313424 ) ) ;
#3811 = CARTESIAN_POINT ( 'NONE',  ( 0.2373612774290684013, -0.1023622047244094474, 0.06430355563125962626 ) ) ;
#3812 = DIRECTION ( 'NONE',  ( 1.000000000000000000, 0.000000000000000000, 3.476578583725179813E-16 ) ) ;
#3813 = CARTESIAN_POINT ( 'NONE',  ( 0.000000000000000000, 1.385826771653543510, 0.000000000000000000 ) ) ;
#3814 = VERTEX_POINT ( 'NONE', #1234 ) ;
#3815 = ORIENTED_EDGE ( 'NONE', *, *, #8873, .F. ) ;
#3816 = EDGE_LOOP ( 'NONE', ( #7841, #5554, #8593, #9327 ) ) ;
#3817 = ORIENTED_EDGE ( 'NONE', *, *, #14916, .T. ) ;
#3818 = ORIENTED_EDGE ( 'NONE', *, *, #4344, .T. ) ;
#3819 = AXIS2_PLACEMENT_3D ( 'NONE', #3578, #9391, #11665 ) ;
#3820 = CARTESIAN_POINT ( 'NONE',  ( -0.5576140732134202693, -0.4881889763779528324, 0.2082870074805209804 ) ) ;
#3821 = DIRECTION ( 'NONE',  ( 0.000000000000000000, 0.000000000000000000, 1.000000000000000000 ) ) ;
#3822 = VECTOR ( 'NONE', #9532, 39.37007874015748143 ) ;
#3823 = FACE_OUTER_BOUND ( 'NONE', #4275, .T. ) ;
#3824 = CARTESIAN_POINT ( 'NONE',  ( -0.4815353412745217998, 1.340095897400991110, 0.3474236500605538125 ) ) ;
#3825 = CARTESIAN_POINT ( 'NONE',  ( -1.895444647785978542, -2.883186813555515648, 0.1048134176421858937 ) ) ;
#3826 = EDGE_LOOP ( 'NONE', ( #8033, #2282, #798, #4253 ) ) ;
#3827 = CARTESIAN_POINT ( 'NONE',  ( -1.972730759285706181, -2.863434052066349711, -0.1336313644289080227 ) ) ;
#3828 = DIRECTION ( 'NONE',  ( 0.000000000000000000, 0.000000000000000000, -1.000000000000000000 ) ) ;
#3829 = DIRECTION ( 'NONE',  ( -1.000000000000000000, -0.000000000000000000, 0.000000000000000000 ) ) ;
#3830 = ORIENTED_EDGE ( 'NONE', *, *, #11516, .T. ) ;
#3831 = EDGE_CURVE ( 'NONE', #2464, #15288, #587, .T. ) ;
#3832 = VERTEX_POINT ( 'NONE', #10773 ) ;
#3833 = CIRCLE ( 'NONE', #12595, 2.795275590551181466 ) ;
#3834 = AXIS2_PLACEMENT_3D ( 'NONE', #11060, #346, #9910 ) ;
#3835 = ADVANCED_FACE ( 'NONE', ( #54 ), #2919, .T. ) ;
#3836 = AXIS2_PLACEMENT_3D ( 'NONE', #5912, #9373, #14236 ) ;
#3837 = EDGE_LOOP ( 'NONE', ( #12569, #8807, #7053 ) ) ;
#3838 = CARTESIAN_POINT ( 'NONE',  ( 0.5084014747882494856, -0.003937007874015747977, 0.2935257283254013583 ) ) ;
#3839 = ADVANCED_FACE ( 'NONE', ( #4898 ), #3734, .F. ) ;
#3840 = CARTESIAN_POINT ( 'NONE',  ( 1.181102362204724310, 4.044111181948214319E-16, 0.02952755905511811330 ) ) ;
#3841 = CARTESIAN_POINT ( 'NONE',  ( 8.630384923125046426E-17, 0.5905511811023621549, 0.7007874015748031260 ) ) ;
#3842 = CIRCLE ( 'NONE', #11595, 0.003937007874015758385 ) ;
#3843 = LINE ( 'NONE', #8713, #13967 ) ;
#3844 = CIRCLE ( 'NONE', #853, 0.003937007874015747109 ) ;
#3845 = CARTESIAN_POINT ( 'NONE',  ( -0.03549374849269303772, -0.1824859222442999918, -0.04671604978335693048 ) ) ;
#3846 = ORIENTED_EDGE ( 'NONE', *, *, #9108, .F. ) ;
#3847 = CARTESIAN_POINT ( 'NONE',  ( 0.2359202325322792559, -0.4881889763779528324, 0.06286251073447048088 ) ) ;
#3848 = CIRCLE ( 'NONE', #10354, 0.5905511811023621549 ) ;
#3849 = LINE ( 'NONE', #12171, #6839 ) ;
#3850 = CIRCLE ( 'NONE', #12615, 0.007874015748031516770 ) ;
#3851 = DIRECTION ( 'NONE',  ( -4.865806668049467791E-32, 1.000000000000000000, 1.224646799147353207E-16 ) ) ;
#3852 = EDGE_CURVE ( 'NONE', #12093, #9857, #9098, .T. ) ;
#3853 = ADVANCED_FACE ( 'NONE', ( #3230 ), #10124, .T. ) ;
#3854 = EDGE_LOOP ( 'NONE', ( #1220, #1766, #922, #11113 ) ) ;
#3855 = EDGE_LOOP ( 'NONE', ( #10494, #6517, #8875, #5036 ) ) ;
#3857 = EDGE_LOOP ( 'NONE', ( #1116, #7494, #22, #3642 ) ) ;
#3856 = AXIS2_PLACEMENT_3D ( 'NONE', #11426, #6711, #703 ) ;
#3858 = TOROIDAL_SURFACE ( 'NONE', #866, 0.1240157480314959815, 0.003937007874015747977 ) ;
#3859 = ORIENTED_EDGE ( 'NONE', *, *, #3227, .T. ) ;
#3860 = AXIS2_PLACEMENT_3D ( 'NONE', #4384, #12704, #1968 ) ;
#3861 = EDGE_CURVE ( 'NONE', #12353, #5050, #791, .T. ) ;
#3862 = AXIS2_PLACEMENT_3D ( 'NONE', #5311, #7129, #1197 ) ;
#3863 = LINE ( 'NONE', #8793, #6384 ) ;
#3864 = CARTESIAN_POINT ( 'NONE',  ( 8.148240514011916814E-17, 1.417322834645669438, 0.6614173228346456046 ) ) ;
#3865 = AXIS2_PLACEMENT_3D ( 'NONE', #1061, #15404, #4668 ) ;
#3866 = CARTESIAN_POINT ( 'NONE',  ( -1.964126537190517885, -2.749515453455440905, 0.1756903148397125081 ) ) ;
#3867 = SPHERICAL_SURFACE ( 'NONE', #837, 0.003937007874015747977 ) ;
#3868 = DIRECTION ( 'NONE',  ( -0.4356761836762390594, 0.8642424528470444844, 0.2515377619249880570 ) ) ;
#3869 = CARTESIAN_POINT ( 'NONE',  ( 2.419703784132994590E-19, 0.07093549527207483607, -0.07900545476875228679 ) ) ;
#3870 = CARTESIAN_POINT ( 'NONE',  ( -2.184126211765464287, -1.725292181286298021, 0.08417626406393743932 ) ) ;
#3871 = DIRECTION ( 'NONE',  ( -0.000000000000000000, -1.000000000000000000, -0.000000000000000000 ) ) ;
#3872 = DIRECTION ( 'NONE',  ( 0.000000000000000000, 0.000000000000000000, 1.000000000000000000 ) ) ;
#3873 = CARTESIAN_POINT ( 'NONE',  ( 0.000000000000000000, 1.409448818897637956, 0.000000000000000000 ) ) ;
#3874 = AXIS2_PLACEMENT_3D ( 'NONE', #31, #3777, #9573 ) ;
#3875 = AXIS2_PLACEMENT_3D ( 'NONE', #11300, #2842, #13571 ) ;
#3876 = VECTOR ( 'NONE', #1023, 39.37007874015748143 ) ;
#3877 = DIRECTION ( 'NONE',  ( -0.000000000000000000, -1.000000000000000000, -0.000000000000000000 ) ) ;
#3878 = AXIS2_PLACEMENT_3D ( 'NONE', #4467, #15278, #3368 ) ;
#3879 = ADVANCED_FACE ( 'NONE', ( #7924 ), #4303, .T. ) ;
#3880 = EDGE_LOOP ( 'NONE', ( #11580, #94, #4442, #4403 ) ) ;
#3881 = EDGE_LOOP ( 'NONE', ( #586, #11289, #1609, #11068 ) ) ;
#3882 = EDGE_LOOP ( 'NONE', ( #11977, #1304, #2598 ) ) ;
#3883 = EDGE_CURVE ( 'NONE', #13232, #4530, #5553, .T. ) ;
#3884 = AXIS2_PLACEMENT_3D ( 'NONE', #9319, #3369, #2201 ) ;
#3885 = AXIS2_PLACEMENT_3D ( 'NONE', #2453, #7229, #14815 ) ;
#3886 = AXIS2_PLACEMENT_3D ( 'NONE', #6337, #2754, #14756 ) ;
#3887 = AXIS2_PLACEMENT_3D ( 'NONE', #2763, #14458, #6124 ) ;
#3888 = DIRECTION ( 'NONE',  ( -0.000000000000000000, -1.000000000000000000, -0.000000000000000000 ) ) ;
#3889 = CARTESIAN_POINT ( 'NONE',  ( -1.925556412971271669, -2.948029930094562712, -0.02618410116112765071 ) ) ;
#3890 = CARTESIAN_POINT ( 'NONE',  ( 0.000000000000000000, 0.000000000000000000, 0.000000000000000000 ) ) ;
#3891 = CONICAL_SURFACE ( 'NONE', #11647, 0.05298991407461853265, 1.279339532317029349 ) ;
#3892 = DIRECTION ( 'NONE',  ( 0.000000000000000000, 0.000000000000000000, 1.000000000000000000 ) ) ;
#3893 = EDGE_CURVE ( 'NONE', #7930, #15252, #2334, .T. ) ;
#3894 = DIRECTION ( 'NONE',  ( 1.000000000000000000, 0.000000000000000000, -0.000000000000000000 ) ) ;
#3895 = DIRECTION ( 'NONE',  ( -0.5000000000000004441, 0.000000000000000000, 0.8660254037844383745 ) ) ;
#3896 = DIRECTION ( 'NONE',  ( -0.000000000000000000, -1.000000000000000000, -0.000000000000000000 ) ) ;
#3897 = CARTESIAN_POINT ( 'NONE',  ( -1.926734873413887383, -2.799953544547113538, 0.1540989716193912062 ) ) ;
#3898 = DIRECTION ( 'NONE',  ( -0.000000000000000000, -1.000000000000000000, -0.000000000000000000 ) ) ;
#3899 = CARTESIAN_POINT ( 'NONE',  ( 0.4828087445803717070, 1.339342401112375125, 0.3474236500605413780 ) ) ;
#3900 = AXIS2_PLACEMENT_3D ( 'NONE', #10004, #3896, #8676 ) ;
#3901 = VECTOR ( 'NONE', #3747, 39.37007874015748143 ) ;
#3902 = CIRCLE ( 'NONE', #5385, 0.1574803149606299191 ) ;
#3903 = ORIENTED_EDGE ( 'NONE', *, *, #9121, .F. ) ;
#3904 = ORIENTED_EDGE ( 'NONE', *, *, #10075, .F. ) ;
#3905 = ORIENTED_EDGE ( 'NONE', *, *, #4166, .F. ) ;
#3906 = AXIS2_PLACEMENT_3D ( 'NONE', #1311, #8355, #13141 ) ;
#3907 = ORIENTED_EDGE ( 'NONE', *, *, #12859, .T. ) ;
#3908 = ORIENTED_EDGE ( 'NONE', *, *, #12241, .T. ) ;
#3909 = DIRECTION ( 'NONE',  ( 0.000000000000000000, 0.000000000000000000, -1.000000000000000000 ) ) ;
#3910 = CARTESIAN_POINT ( 'NONE',  ( 0.000000000000000000, 0.3464566929133857109, -0.5511811023622046335 ) ) ;
#3911 = CIRCLE ( 'NONE', #5406, 0.5433070866141731514 ) ;
#3912 = DIRECTION ( 'NONE',  ( -1.000000000000000000, 8.673617379884035472E-15, -0.000000000000000000 ) ) ;
#3913 = ADVANCED_FACE ( 'NONE', ( #1809 ), #11598, .T. ) ;
#3914 = CARTESIAN_POINT ( 'NONE',  ( -1.992382107315058271, -2.749515453455440905, 0.1756903148397124803 ) ) ;
#3915 = CARTESIAN_POINT ( 'NONE',  ( -0.4787092522273656559, 1.341768146560826214, 0.3474236500605662470 ) ) ;
#3916 = CIRCLE ( 'NONE', #1417, 0.003937007874015741038 ) ;
#3917 = CARTESIAN_POINT ( 'NONE',  ( -1.880695783986644498, -2.919830138821126297, -0.02855755338539034058 ) ) ;
#3918 = ORIENTED_EDGE ( 'NONE', *, *, #12662, .F. ) ;
#3919 = CARTESIAN_POINT ( 'NONE',  ( 0.4307978335858664853, -0.09842519685039370636, 0.4279391777402732910 ) ) ;
#3920 = DIRECTION ( 'NONE',  ( -1.000000000000000000, 0.000000000000000000, 0.000000000000000000 ) ) ;
#3921 = DIRECTION ( 'NONE',  ( -0.4999999999999996114, -0.000000000000000000, -0.8660254037844389297 ) ) ;
#3922 = ORIENTED_EDGE ( 'NONE', *, *, #10347, .T. ) ;
#3923 = ORIENTED_EDGE ( 'NONE', *, *, #9756, .F. ) ;
#3924 = AXIS2_PLACEMENT_3D ( 'NONE', #4656, #3487, #8259 ) ;
#3925 = ORIENTED_EDGE ( 'NONE', *, *, #8096, .T. ) ;
#3926 = AXIS2_PLACEMENT_3D ( 'NONE', #7830, #7758, #12548 ) ;
#3927 = DIRECTION ( 'NONE',  ( 0.000000000000000000, 1.000000000000000000, 0.000000000000000000 ) ) ;
#3928 = DIRECTION ( 'NONE',  ( 0.5984233124757303290, 0.8011800915434521553, 0.000000000000000000 ) ) ;
#3929 = CARTESIAN_POINT ( 'NONE',  ( -0.4783464566929145900, -0.1023622047244094474, 0.3534565624369550574 ) ) ;
#3930 = DIRECTION ( 'NONE',  ( 0.8011800915434506010, -0.5984233124757325495, 0.000000000000000000 ) ) ;
#3931 = PLANE ( 'NONE',  #13392 ) ;
#3932 = ORIENTED_EDGE ( 'NONE', *, *, #6134, .F. ) ;
#3933 = CARTESIAN_POINT ( 'NONE',  ( 7.232166136696967594E-17, 0.000000000000000000, 0.5905511811023621549 ) ) ;
#3934 = DIRECTION ( 'NONE',  ( 0.000000000000000000, -0.000000000000000000, -1.000000000000000000 ) ) ;
#3935 = SPHERICAL_SURFACE ( 'NONE', #15152, 0.003937007874015747977 ) ;
#3936 = TOROIDAL_SURFACE ( 'NONE', #10933, 0.6614173228346456046, 0.007874015748031495954 ) ;
#3937 = CARTESIAN_POINT ( 'NONE',  ( -0.04507696108106435534, -0.1650637432014245565, 0.05202626060216886117 ) ) ;
#3938 = EDGE_CURVE ( 'NONE', #10200, #4047, #14354, .T. ) ;
#3939 = PRODUCT_DEFINITION_SHAPE ( 'NONE', 'NONE',  #15480 ) ;
#3940 = CARTESIAN_POINT ( 'NONE',  ( -2.755905511811024056, 0.2985367441494412022, -0.1033464566929133965 ) ) ;
#3941 = AXIS2_PLACEMENT_3D ( 'NONE', #10111, #4156, #4386 ) ;
#3942 = ORIENTED_EDGE ( 'NONE', *, *, #7006, .T. ) ;
#3943 = ORIENTED_EDGE ( 'NONE', *, *, #3193, .T. ) ;
#3944 = CIRCLE ( 'NONE', #12709, 0.007874015748031482076 ) ;
#3945 = ORIENTED_EDGE ( 'NONE', *, *, #15043, .F. ) ;
#3946 = CYLINDRICAL_SURFACE ( 'NONE', #9423, 0.03937007874015751446 ) ;
#3947 = DIRECTION ( 'NONE',  ( 0.4999999999999977240, -1.084202172485506012E-15, -0.8660254037844400399 ) ) ;
#3948 = VECTOR ( 'NONE', #8091, 39.37007874015748143 ) ;
#3949 = EDGE_CURVE ( 'NONE', #9786, #14935, #13961, .T. ) ;
#3950 = CARTESIAN_POINT ( 'NONE',  ( -2.096257313159167968, -1.821548935441466677, 0.1033814208906759513 ) ) ;
#3951 = CARTESIAN_POINT ( 'NONE',  ( 1.181102362204724310, 0.1240157480314963978, 0.02559055118110236185 ) ) ;
#3952 = DIRECTION ( 'NONE',  ( 3.053113317719180486E-16, 0.9706086590632808653, 0.2406633145109156047 ) ) ;
#3953 = CARTESIAN_POINT ( 'NONE',  ( -1.419029514950140625, -0.01190400850868964661, 0.07305840954582080993 ) ) ;
#3954 = ADVANCED_FACE ( 'NONE', ( #7998 ), #10204, .T. ) ;
#3955 = CARTESIAN_POINT ( 'NONE',  ( 7.232166136696967594E-17, 1.370078740157480546, 0.5905511811023621549 ) ) ;
#3956 = CYLINDRICAL_SURFACE ( 'NONE', #8398, 0.5905511811023621549 ) ;
#3957 = DIRECTION ( 'NONE',  ( -0.000000000000000000, -1.000000000000000000, 0.000000000000000000 ) ) ;
#3958 = DIRECTION ( 'NONE',  ( 0.000000000000000000, 0.000000000000000000, 1.000000000000000000 ) ) ;
#3959 = VECTOR ( 'NONE', #3371, 39.37007874015748143 ) ;
#3960 = EDGE_CURVE ( 'NONE', #8067, #10377, #3296, .T. ) ;
#3961 = DIRECTION ( 'NONE',  ( 0.8660254037844362651, 0.000000000000000000, -0.5000000000000041078 ) ) ;
#3962 = ORIENTED_EDGE ( 'NONE', *, *, #8579, .T. ) ;
#3963 = AXIS2_PLACEMENT_3D ( 'NONE', #12480, #11286, #2918 ) ;
#3964 = VERTEX_POINT ( 'NONE', #12629 ) ;
#3965 = DIRECTION ( 'NONE',  ( 0.000000000000000000, 0.000000000000000000, 1.000000000000000000 ) ) ;
#3966 = ORIENTED_EDGE ( 'NONE', *, *, #3521, .T. ) ;
#3967 = ORIENTED_EDGE ( 'NONE', *, *, #1933, .T. ) ;
#3968 = AXIS2_PLACEMENT_3D ( 'NONE', #7123, #3603, #9320 ) ;
#3969 = EDGE_CURVE ( 'NONE', #14915, #9786, #4838, .T. ) ;
#3970 = LINE ( 'NONE', #8905, #9357 ) ;
#3971 = CARTESIAN_POINT ( 'NONE',  ( -1.935472858800945994, -2.920743354953669879, 0.09758401094301728806 ) ) ;
#3972 = DIRECTION ( 'NONE',  ( 0.000000000000000000, 0.000000000000000000, 1.000000000000000000 ) ) ;
#3973 = ADVANCED_FACE ( 'NONE', ( #11692 ), #963, .F. ) ;
#3974 = CARTESIAN_POINT ( 'NONE',  ( -1.181846040523323538, 0.3414510609348502257, -0.04963317811004215596 ) ) ;
#3975 = DIRECTION ( 'NONE',  ( 0.000000000000000000, 0.000000000000000000, -1.000000000000000000 ) ) ;
#3976 = LINE ( 'NONE', #14630, #15084 ) ;
#3977 = CARTESIAN_POINT ( 'NONE',  ( -0.09948011493072102251, -0.4921259842519685179, -0.2443248468741946733 ) ) ;
#3978 = CARTESIAN_POINT ( 'NONE',  ( -1.898348652445378981, -2.875798882032482240, 0.1126135460449128739 ) ) ;
#3979 = EDGE_CURVE ( 'NONE', #9040, #12795, #5073, .T. ) ;
#3980 = DIRECTION ( 'NONE',  ( 0.000000000000000000, 0.000000000000000000, -1.000000000000000000 ) ) ;
#3981 = DIRECTION ( 'NONE',  ( 0.000000000000000000, 0.000000000000000000, -1.000000000000000000 ) ) ;
#3982 = EDGE_CURVE ( 'NONE', #12461, #692, #6837, .T. ) ;
#3983 = ORIENTED_EDGE ( 'NONE', *, *, #15011, .T. ) ;
#3984 = ORIENTED_EDGE ( 'NONE', *, *, #12469, .F. ) ;
#3985 = ORIENTED_EDGE ( 'NONE', *, *, #2335, .F. ) ;
#3986 = ORIENTED_EDGE ( 'NONE', *, *, #1585, .T. ) ;
#3987 = VERTEX_POINT ( 'NONE', #3062 ) ;
#3988 = CARTESIAN_POINT ( 'NONE',  ( -1.415641383055952440, -0.01001468546970056897, -0.06638871894587755618 ) ) ;
#3989 = CARTESIAN_POINT ( 'NONE',  ( -1.599731447215819058, 0.1084887237744113775, 0.04822519498664557674 ) ) ;
#3990 = DIRECTION ( 'NONE',  ( 8.673617379884035472E-15, 1.000000000000000000, 0.000000000000000000 ) ) ;
#3991 = FACE_OUTER_BOUND ( 'NONE', #4826, .T. ) ;
#3992 = CARTESIAN_POINT ( 'NONE',  ( 0.000000000000000000, 1.645669291338583085, -0.7086614173228346081 ) ) ;
#3993 = FACE_BOUND ( 'NONE', #452, .T. ) ;
#3994 = CARTESIAN_POINT ( 'NONE',  ( -1.873911309327628949, -2.936534521027843070, -0.06698651620721371436 ) ) ;
#3995 = ORIENTED_EDGE ( 'NONE', *, *, #14260, .T. ) ;
#3996 = CARTESIAN_POINT ( 'NONE',  ( -2.176528721281673739, -2.014897391718464714, -0.1098265554925635934 ) ) ;
#3997 = DIRECTION ( 'NONE',  ( 0.4999999999999998890, 0.000000000000000000, 0.8660254037844385966 ) ) ;
#3998 = ADVANCED_FACE ( 'NONE', ( #7835 ), #1898, .F. ) ;
#3999 = DIRECTION ( 'NONE',  ( -0.000000000000000000, -1.000000000000000000, -0.000000000000000000 ) ) ;
#4000 = ORIENTED_EDGE ( 'NONE', *, *, #13102, .F. ) ;
#4001 = EDGE_LOOP ( 'NONE', ( #7465, #8050, #13852, #3492 ) ) ;
#4002 = ADVANCED_FACE ( 'NONE', ( #3381 ), #7049, .F. ) ;
#4003 = EDGE_CURVE ( 'NONE', #9812, #9857, #3729, .T. ) ;
#4004 = ORIENTED_EDGE ( 'NONE', *, *, #11604, .T. ) ;
#4005 = LINE ( 'NONE', #8709, #5328 ) ;
#4006 = DIRECTION ( 'NONE',  ( 0.000000000000000000, -1.000000000000000000, 0.000000000000000000 ) ) ;
#4007 = CARTESIAN_POINT ( 'NONE',  ( 0.5379290338433416752, -0.09448818897637796532, 0.2423824958184915834 ) ) ;
#4008 = CYLINDRICAL_SURFACE ( 'NONE', #14725, 0.07874015748031495954 ) ;
#4009 = CARTESIAN_POINT ( 'NONE',  ( -0.02015118043373552090, -0.1802412052441877965, -0.0009776059035733464502 ) ) ;
#4010 = ORIENTED_EDGE ( 'NONE', *, *, #13995, .F. ) ;
#4011 = CARTESIAN_POINT ( 'NONE',  ( 0.7205731843802273273, 1.190944881889763884, 0.4842140986486808130 ) ) ;
#4012 = FACE_OUTER_BOUND ( 'NONE', #469, .T. ) ;
#4013 = CARTESIAN_POINT ( 'NONE',  ( -0.02281238468002976319, -0.1806356120156163148, 0.007039490205851098130 ) ) ;
#4014 = FACE_OUTER_BOUND ( 'NONE', #1961, .T. ) ;
#4015 = ORIENTED_EDGE ( 'NONE', *, *, #1981, .F. ) ;
#4016 = ORIENTED_EDGE ( 'NONE', *, *, #13802, .T. ) ;
#4017 = CARTESIAN_POINT ( 'NONE',  ( 0.05905511811023622659, 1.043307086614173151, -0.8267716535433072833 ) ) ;
#4018 = CARTESIAN_POINT ( 'NONE',  ( -0.2661821753646866906, -0.4921259842519685179, 0.03548265769538203052 ) ) ;
#4019 = DIRECTION ( 'NONE',  ( -3.614007241618347785E-16, 0.000000000000000000, 1.000000000000000000 ) ) ;
#4020 = DIRECTION ( 'NONE',  ( 8.673617379884028076E-17, 1.000000000000000000, 0.000000000000000000 ) ) ;
#4021 = DIRECTION ( 'NONE',  ( 0.5000000000000038858, 1.641048408274059511E-15, -0.8660254037844363761 ) ) ;
#4022 = PLANE ( 'NONE',  #358 ) ;
#4023 = LINE ( 'NONE', #11388, #10675 ) ;
#4024 = DIRECTION ( 'NONE',  ( -1.000000000000000000, -0.000000000000000000, -3.973232667114495301E-16 ) ) ;
#4025 = FACE_OUTER_BOUND ( 'NONE', #2925, .T. ) ;
#4026 = CARTESIAN_POINT ( 'NONE',  ( -0.2364476915723336681, -0.4881889763779528324, 0.06377609659094583827 ) ) ;
#4027 = ORIENTED_EDGE ( 'NONE', *, *, #11140, .F. ) ;
#4028 = ADVANCED_FACE ( 'NONE', ( #8160 ), #8305, .T. ) ;
#4029 = VERTEX_POINT ( 'NONE', #10577 ) ;
#4030 = EDGE_CURVE ( 'NONE', #13855, #7381, #10506, .T. ) ;
#4031 = VERTEX_POINT ( 'NONE', #9500 ) ;
#4032 = EDGE_CURVE ( 'NONE', #15013, #8301, #15350, .T. ) ;
#4033 = DIRECTION ( 'NONE',  ( -0.8144815189573204606, 0.5801894994542525774, -1.283760644411384396E-16 ) ) ;
#4034 = CARTESIAN_POINT ( 'NONE',  ( -1.935621620635804785, -2.920307329271410790, -0.09762439764854415059 ) ) ;
#4035 = DIRECTION ( 'NONE',  ( -0.000000000000000000, -1.000000000000000000, -0.000000000000000000 ) ) ;
#4036 = CARTESIAN_POINT ( 'NONE',  ( -0.09842519685028340570, -0.4881889763779528324, -0.5870514566507987197 ) ) ;
#4037 = CARTESIAN_POINT ( 'NONE',  ( 0.5649606299212333038, -0.09448818897637796532, 0.2034364137499355130 ) ) ;
#4038 = FACE_OUTER_BOUND ( 'NONE', #9060, .T. ) ;
#4039 = CARTESIAN_POINT ( 'NONE',  ( -0.01089193232087468620, -0.1772239411783215757, 5.880576042184872077E-16 ) ) ;
#4040 = DIRECTION ( 'NONE',  ( 0.5801894994542512451, 0.8144815189573213488, 0.000000000000000000 ) ) ;
#4041 = CARTESIAN_POINT ( 'NONE',  ( 0.000000000000000000, 2.165354330708661568, 0.000000000000000000 ) ) ;
#4042 = ORIENTED_EDGE ( 'NONE', *, *, #901, .F. ) ;
#4043 = EDGE_CURVE ( 'NONE', #1436, #563, #8241, .T. ) ;
#4044 = EDGE_LOOP ( 'NONE', ( #5367, #10990, #9323, #1073 ) ) ;
#4045 = EDGE_LOOP ( 'NONE', ( #4859, #4571 ) ) ;
#4046 = EDGE_CURVE ( 'NONE', #13544, #9837, #4545, .T. ) ;
#4047 = VERTEX_POINT ( 'NONE', #9420 ) ;
#4048 = ORIENTED_EDGE ( 'NONE', *, *, #9169, .T. ) ;
#4049 = CARTESIAN_POINT ( 'NONE',  ( -1.404141343084615912, -0.005156784085991158832, -0.05951157569786713619 ) ) ;
#4050 = EDGE_CURVE ( 'NONE', #7774, #9271, #10599, .T. ) ;
#4051 = DIRECTION ( 'NONE',  ( 0.5000000000000035527, 0.000000000000000000, -0.8660254037844365982 ) ) ;
#4052 = CARTESIAN_POINT ( 'NONE',  ( -1.592259916642357442, 0.1190110821474778119, 0.06350111023902092755 ) ) ;
#4053 = CARTESIAN_POINT ( 'NONE',  ( 0.000000000000000000, 2.433070866141732846, 0.000000000000000000 ) ) ;
#4054 = CYLINDRICAL_SURFACE ( 'NONE', #1122, 0.003937007874015741038 ) ;
#4055 = CARTESIAN_POINT ( 'NONE',  ( 0.000000000000000000, 1.606299212598425674, -0.6692913385826770867 ) ) ;
#4056 = CARTESIAN_POINT ( 'NONE',  ( 0.000000000000000000, 2.433070866141732846, -0.5826771653543306728 ) ) ;
#4057 = CARTESIAN_POINT ( 'NONE',  ( -1.883471559757083913, -2.913266620391066208, 0.1077232328358656566 ) ) ;
#4058 = ORIENTED_EDGE ( 'NONE', *, *, #13630, .T. ) ;
#4059 = DIRECTION ( 'NONE',  ( 0.000000000000000000, 0.000000000000000000, 1.000000000000000000 ) ) ;
#4060 = CARTESIAN_POINT ( 'NONE',  ( 0.000000000000000000, 0.5905511811023621549, 0.000000000000000000 ) ) ;
#4061 = VERTEX_POINT ( 'NONE', #3343 ) ;
#4062 = ORIENTED_EDGE ( 'NONE', *, *, #7538, .F. ) ;
#4063 = ADVANCED_FACE ( 'NONE', ( #15259 ), #12097, .F. ) ;
#4064 = UNCERTAINTY_MEASURE_WITH_UNIT (LENGTH_MEASURE( 1.000000000000000082E-05 ), #421, 'distance_accuracy_value', 'NONE');
#4065 = EDGE_LOOP ( 'NONE', ( #3945, #7797, #8415, #10493 ) ) ;
#4066 = TOROIDAL_SURFACE ( 'NONE', #12585, 0.03543307086614173179, 0.003937007874015747977 ) ;
#4067 = EDGE_CURVE ( 'NONE', #14427, #6389, #12598, .T. ) ;
#4068 = EDGE_CURVE ( 'NONE', #646, #1731, #4518, .T. ) ;
#4069 = DIRECTION ( 'NONE',  ( 0.000000000000000000, 0.000000000000000000, -1.000000000000000000 ) ) ;
#4070 = DIRECTION ( 'NONE',  ( 0.7402970580929170152, 0.6722799013647308142, 0.000000000000000000 ) ) ;
#4071 = CARTESIAN_POINT ( 'NONE',  ( -1.063205505495480097, 0.7941372572243097228, -0.03937007874015747977 ) ) ;
#4072 = CARTESIAN_POINT ( 'NONE',  ( 0.5445274672588121812, 1.338626482899105241, 0.2461921031270739857 ) ) ;
#4073 = ORIENTED_EDGE ( 'NONE', *, *, #7538, .T. ) ;
#4074 = FACE_OUTER_BOUND ( 'NONE', #4736, .T. ) ;
#4075 = ADVANCED_FACE ( 'NONE', ( #14073 ), #11871, .T. ) ;
#4076 = CARTESIAN_POINT ( 'NONE',  ( -0.07874015748031520934, 1.062385330869439640E-16, 0.05905511811023622659 ) ) ;
#4077 = CARTESIAN_POINT ( 'NONE',  ( -0.1062992125983150127, -0.1023622047244094474, -0.2482618547482104421 ) ) ;
#4078 = AXIS2_PLACEMENT_3D ( 'NONE', #615, #6182, #12163 ) ;
#4079 = AXIS2_PLACEMENT_3D ( 'NONE', #4502, #14064, #8333 ) ;
#4080 = CARTESIAN_POINT ( 'NONE',  ( -0.4828087445803670441, 1.339342401112374903, 0.3474236500605482614 ) ) ;
#4081 = AXIS2_PLACEMENT_3D ( 'NONE', #5676, #9291, #14155 ) ;
#4082 = FACE_OUTER_BOUND ( 'NONE', #14179, .T. ) ;
#4083 = AXIS2_PLACEMENT_3D ( 'NONE', #10799, #12458, #14880 ) ;
#4084 = ORIENTED_EDGE ( 'NONE', *, *, #3429, .T. ) ;
#4085 = B_SPLINE_CURVE_WITH_KNOTS ( 'NONE', 3,
 ( #4451, #15031, #12823, #4281 ),
 .UNSPECIFIED., .F., .F.,
 ( 4, 4 ),
 ( 1.734723475976807094E-18, 2.119993237936608501E-05 ),
 .UNSPECIFIED. ) ;
#4086 = ORIENTED_EDGE ( 'NONE', *, *, #9481, .T. ) ;
#4087 =( REPRESENTATION_RELATIONSHIP ('NONE','NONE', #8904, #7785 ) REPRESENTATION_RELATIONSHIP_WITH_TRANSFORMATION ( #2677 )SHAPE_REPRESENTATION_RELATIONSHIP( ) );
#4088 = CARTESIAN_POINT ( 'NONE',  ( -0.5860051159906336515, -0.09842519685039370636, 0.1591122789105256508 ) ) ;
#4089 = DIRECTION ( 'NONE',  ( 0.5000000000000041078, -0.000000000000000000, 0.8660254037844363761 ) ) ;
#4090 = CIRCLE ( 'NONE', #12611, 0.5905511811023621549 ) ;
#4091 = AXIS2_PLACEMENT_3D ( 'NONE', #4340, #9140, #1844 ) ;
#4092 = AXIS2_PLACEMENT_3D ( 'NONE', #10740, #10668, #9326 ) ;
#4093 = CARTESIAN_POINT ( 'NONE',  ( 0.3137366569588399545, -0.2952755905511811330, 0.2947875711430715251 ) ) ;
#4094 = CARTESIAN_POINT ( 'NONE',  ( -0.2796411686208687963, -0.2952755905511811330, 0.2751025317729920427 ) ) ;
#4095 = AXIS2_PLACEMENT_3D ( 'NONE', #11389, #671, #5427 ) ;
#4096 = DIRECTION ( 'NONE',  ( -0.000000000000000000, -0.000000000000000000, 1.000000000000000000 ) ) ;
#4097 = CARTESIAN_POINT ( 'NONE',  ( -0.1023622047242991467, -0.4881889763779528324, -0.5870514566507987197 ) ) ;
#4098 = EDGE_CURVE ( 'NONE', #8667, #2746, #7338, .T. ) ;
#4099 = DIRECTION ( 'NONE',  ( 0.5000000000000001110, -0.000000000000000000, -0.8660254037844385966 ) ) ;
#4100 = DIRECTION ( 'NONE',  ( 0.000000000000000000, 0.000000000000000000, 1.000000000000000000 ) ) ;
#4101 = DIRECTION ( 'NONE',  ( 0.9453712468369984689, 0.3259957141648626711, 0.000000000000000000 ) ) ;
#4102 = AXIS2_PLACEMENT_3D ( 'NONE', #2971, #7739, #14963 ) ;
#4103 = CIRCLE ( 'NONE', #4342, 0.007874015748031482076 ) ;
#4104 = ORIENTED_EDGE ( 'NONE', *, *, #3703, .T. ) ;
#4105 = FACE_OUTER_BOUND ( 'NONE', #6408, .T. ) ;
#4106 = AXIS2_PLACEMENT_3D ( 'NONE', #1957, #2895, #5532 ) ;
#4107 = EDGE_LOOP ( 'NONE', ( #7379, #13511, #11346, #2397 ) ) ;
#4108 = CIRCLE ( 'NONE', #3615, 0.03937007874015761161 ) ;
#4109 = ORIENTED_EDGE ( 'NONE', *, *, #7108, .F. ) ;
#4110 = AXIS2_PLACEMENT_3D ( 'NONE', #7168, #11965, #4887 ) ;
#4111 = DIRECTION ( 'NONE',  ( -0.000000000000000000, -1.000000000000000000, 0.000000000000000000 ) ) ;
#4112 = CARTESIAN_POINT ( 'NONE',  ( -1.972615538042427286, -2.863733741840190028, 0.1334472478180623312 ) ) ;
#4113 = CIRCLE ( 'NONE', #14641, 0.003937007874015758385 ) ;
#4114 = VECTOR ( 'NONE', #13930, 39.37007874015748143 ) ;
#4115 = DIRECTION ( 'NONE',  ( 0.000000000000000000, -1.000000000000000000, 0.000000000000000000 ) ) ;
#4116 = AXIS2_PLACEMENT_3D ( 'NONE', #6971, #4534, #858 ) ;
#4117 = CARTESIAN_POINT ( 'NONE',  ( 0.4751993499420012479, 1.035433070866141891, 0.3506226965216235336 ) ) ;
#4118 = DIRECTION ( 'NONE',  ( -0.8660254037844422603, -0.000000000000000000, 0.4999999999999939493 ) ) ;
#4119 = AXIS2_PLACEMENT_3D ( 'NONE', #12308, #6252, #11125 ) ;
#4120 = DIRECTION ( 'NONE',  ( 1.000000000000000000, 0.000000000000000000, 0.000000000000000000 ) ) ;
#4121 = CARTESIAN_POINT ( 'NONE',  ( -1.908282260581757761, -2.850014880722915755, -0.1332367027562576245 ) ) ;
#4122 = LINE ( 'NONE', #1849, #10328 ) ;
#4123 = DIRECTION ( 'NONE',  ( -0.000000000000000000, -1.000000000000000000, -0.000000000000000000 ) ) ;
#4124 = VERTEX_POINT ( 'NONE', #9529 ) ;
#4125 = EDGE_CURVE ( 'NONE', #4401, #12819, #11351, .T. ) ;
#4126 = ORIENTED_EDGE ( 'NONE', *, *, #11173, .T. ) ;
#4127 = EDGE_LOOP ( 'NONE', ( #11022, #1630, #4130, #223 ) ) ;
#4128 = CIRCLE ( 'NONE', #10633, 0.01968503937007875723 ) ;
#4129 = ORIENTED_EDGE ( 'NONE', *, *, #14675, .T. ) ;
#4130 = ORIENTED_EDGE ( 'NONE', *, *, #13553, .F. ) ;
#4131 = AXIS2_PLACEMENT_3D ( 'NONE', #7207, #13301, #10732 ) ;
#4132 = CYLINDRICAL_SURFACE ( 'NONE', #11393, 0.003937007874015749712 ) ;
#4133 = CYLINDRICAL_SURFACE ( 'NONE', #5820, 0.003937007874015758385 ) ;
#4134 = CARTESIAN_POINT ( 'NONE',  ( -1.590519080053494516, 0.1214231549357709661, 0.06175753274847662483 ) ) ;
#4135 = DIRECTION ( 'NONE',  ( -0.000000000000000000, -1.000000000000000000, -0.000000000000000000 ) ) ;
#4136 = CARTESIAN_POINT ( 'NONE',  ( -0.03886060139087894189, 0.000000000000000000, -0.08219815605944147396 ) ) ;
#4137 = CARTESIAN_POINT ( 'NONE',  ( 0.1657884745773951785, -0.4921259842519685179, 0.2093696482190284258 ) ) ;
#4138 = EDGE_CURVE ( 'NONE', #9448, #6660, #2105, .T. ) ;
#4139 = LINE ( 'NONE', #6544, #9348 ) ;
#4140 = AXIS2_PLACEMENT_3D ( 'NONE', #14483, #2255, #12917 ) ;
#4141 = CARTESIAN_POINT ( 'NONE',  ( -1.181096721277162365, 0.3434326092093347715, 0.03937007874014959025 ) ) ;
#4142 = VECTOR ( 'NONE', #13064, 39.37007874015748143 ) ;
#4143 = CARTESIAN_POINT ( 'NONE',  ( -1.873991930927511040, -2.936340581383783732, 0.06745920558762338870 ) ) ;
#4144 = ADVANCED_FACE ( 'NONE', ( #8202 ), #11966, .F. ) ;
#4145 = AXIS2_PLACEMENT_3D ( 'NONE', #13562, #5325, #7768 ) ;
#4146 = VERTEX_POINT ( 'NONE', #7080 ) ;
#4147 = AXIS2_PLACEMENT_3D ( 'NONE', #997, #5745, #11968 ) ;
#4148 = EDGE_LOOP ( 'NONE', ( #2153, #5372, #12996, #9147 ) ) ;
#4149 = ADVANCED_FACE ( 'NONE', ( #10538 ), #1228, .F. ) ;
#4150 = EDGE_LOOP ( 'NONE', ( #4768, #11696, #4789, #3516 ) ) ;
#4152 = ORIENTED_EDGE ( 'NONE', *, *, #10937, .F. ) ;
#4151 = VECTOR ( 'NONE', #14995, 39.37007874015748143 ) ;
#4153 = AXIS2_PLACEMENT_3D ( 'NONE', #10288, #1595, #14928 ) ;
#4154 = CARTESIAN_POINT ( 'NONE',  ( 0.000000000000000000, 1.346456692913385877, 0.000000000000000000 ) ) ;
#4155 = CARTESIAN_POINT ( 'NONE',  ( 0.06692913385832209572, -0.1023622047244094474, -0.2377126739437405434 ) ) ;
#4156 = DIRECTION ( 'NONE',  ( -0.000000000000000000, 0.000000000000000000, 1.000000000000000000 ) ) ;
#4157 = DIRECTION ( 'NONE',  ( -0.4999999999999998335, 0.000000000000000000, -0.8660254037844388186 ) ) ;
#4158 = CARTESIAN_POINT ( 'NONE',  ( -0.03726694595799353443, -0.1642704670929807653, -0.04781780748315901663 ) ) ;
#4159 = EDGE_CURVE ( 'NONE', #5321, #562, #11878, .T. ) ;
#4160 = EDGE_LOOP ( 'NONE', ( #5101, #9488, #10429, #14250 ) ) ;
#4161 = CARTESIAN_POINT ( 'NONE',  ( -0.1552072824047652233, -0.09448818897637796532, -0.5870514566507987197 ) ) ;
#4162 = CARTESIAN_POINT ( 'NONE',  ( -0.3766253205744463650, -0.2952755905511811330, 0.09924703731238559978 ) ) ;
#4163 = CIRCLE ( 'NONE', #12428, 0.003937007874015737569 ) ;
#4164 = CARTESIAN_POINT ( 'NONE',  ( -0.5894146648244306119, -0.003937007874015747977, 0.1610807828475335490 ) ) ;
#4165 = CARTESIAN_POINT ( 'NONE',  ( -0.2672370934451241409, -0.1023622047244094474, 0.03154564982136626866 ) ) ;
#4166 = EDGE_CURVE ( 'NONE', #8120, #6985, #5087, .T. ) ;
#4167 = CYLINDRICAL_SURFACE ( 'NONE', #5664, 0.003937007874015740171 ) ;
#4168 = CIRCLE ( 'NONE', #7928, 0.03937007874015751446 ) ;
#4169 = EDGE_LOOP ( 'NONE', ( #7404, #5579, #5175, #6829 ) ) ;
#4170 = ORIENTED_EDGE ( 'NONE', *, *, #6509, .F. ) ;
#4171 = ORIENTED_EDGE ( 'NONE', *, *, #3697, .F. ) ;
#4172 = EDGE_CURVE ( 'NONE', #1810, #13131, #1153, .T. ) ;
#4173 = DIRECTION ( 'NONE',  ( 0.000000000000000000, 0.000000000000000000, -1.000000000000000000 ) ) ;
#4174 = FACE_OUTER_BOUND ( 'NONE', #14256, .T. ) ;
#4175 = CARTESIAN_POINT ( 'NONE',  ( -2.100501784635051550, -1.630597114118274238, 0.1033464566929129663 ) ) ;
#4176 = DIRECTION ( 'NONE',  ( -0.000000000000000000, -1.000000000000000000, -0.000000000000000000 ) ) ;
#4177 = PRODUCT_CONTEXT ( 'NONE', #900, 'mechanical' ) ;
#4178 = CARTESIAN_POINT ( 'NONE',  ( 0.000000000000000000, 0.003937007874015860734, 0.000000000000000000 ) ) ;
#4179 = DIRECTION ( 'NONE',  ( 0.000000000000000000, 0.000000000000000000, 1.000000000000000000 ) ) ;
#4180 = CARTESIAN_POINT ( 'NONE',  ( -1.431036756819010769, -0.02829858486107857465, 0.08366141732283458032 ) ) ;
#4181 = AXIS2_PLACEMENT_3D ( 'NONE', #9268, #14047, #2140 ) ;
#4182 = CARTESIAN_POINT ( 'NONE',  ( -0.2953892001169318160, -0.2952755905511811330, 0.2478261411026162764 ) ) ;
#4183 =( BOUNDED_SURFACE ( )  B_SPLINE_SURFACE ( 3, 2, ( 
 ( #5219, #7660, #12524 ),
 ( #8760, #11261, #10015 ),
 ( #13530, #6297, #4049 ),
 ( #9861, #1487, #475 ),
 ( #5285, #13604, #2967 ),
 ( #11094, #2877, #3988 ),
 ( #6236, #6475, #8924 ),
 ( #10082, #14870, #12226 ),
 ( #14648, #388, #1784 ),
 ( #7562, #6394, #12357 ) ),
 .UNSPECIFIED., .F., .F., .T. ) 
 B_SPLINE_SURFACE_WITH_KNOTS ( ( 4, 2, 2, 2, 4 ),
 ( 3, 3 ),
 ( 0.000000000000000000, 0.0004011259949119783835, 0.0008022519898239567670, 0.001203377984735935205, 0.001604503979647913534 ),
 ( 0.000000000000000000, 1.000000000000000000 ),
 .UNSPECIFIED. ) 
 GEOMETRIC_REPRESENTATION_ITEM ( )  RATIONAL_B_SPLINE_SURFACE ( (
 ( 1.000000000000000000, 0.7071067811865476838, 1.000000000000000000),
 ( 1.000000000000000000, 0.6902033478571758529, 1.000000000000000000),
 ( 1.000000000000000000, 0.6755035747093588450, 1.000000000000000000),
 ( 1.000000000000000000, 0.6523092178238821814, 1.000000000000000000),
 ( 1.000000000000000000, 0.6440979550411551902, 1.000000000000000000),
 ( 1.000000000000000000, 0.6332442468201355812, 1.000000000000000000),
 ( 1.000000000000000000, 0.6305611707286850054, 1.000000000000000000),
 ( 1.000000000000000000, 0.6276691513331230654, 1.000000000000000000),
 ( 1.000000000000000000, 0.6273773519528882403, 1.000000000000000000),
 ( 1.000000000000000000, 0.6273322353868016066, 1.000000000000000000) ) ) 
 REPRESENTATION_ITEM ( '' )  SURFACE ( )  );
#4184 = DIRECTION ( 'NONE',  ( 0.000000000000000000, 1.000000000000000000, 0.000000000000000000 ) ) ;
#4185 = ADVANCED_FACE ( 'NONE', ( #3648 ), #14871, .T. ) ;
#4186 = EDGE_LOOP ( 'NONE', ( #7515, #10438, #8783, #11463 ) ) ;
#4187 = CIRCLE ( 'NONE', #2690, 0.003937007874015724558 ) ;
#4188 = ORIENTED_EDGE ( 'NONE', *, *, #1999, .T. ) ;
#4189 = CARTESIAN_POINT ( 'NONE',  ( -0.5615510810874361214, -0.1023622047244094474, 0.2014679098129270318 ) ) ;
#4190 = ORIENTED_EDGE ( 'NONE', *, *, #2152, .T. ) ;
#4191 = AXIS2_PLACEMENT_3D ( 'NONE', #7329, #8448, #3745 ) ;
#4192 = EDGE_CURVE ( 'NONE', #11838, #3552, #13859, .T. ) ;
#4193 = EDGE_LOOP ( 'NONE', ( #4587, #12288, #1894, #11439 ) ) ;
#4194 = EDGE_CURVE ( 'NONE', #5049, #8019, #13054, .T. ) ;
#4195 = CARTESIAN_POINT ( 'NONE',  ( 0.000000000000000000, 0.5826771653543306728, -0.7007874015748031260 ) ) ;
#4196 = CARTESIAN_POINT ( 'NONE',  ( -2.011807227224586825, -2.756102811318747126, 0.1765457041329565879 ) ) ;
#4197 = AXIS2_PLACEMENT_3D ( 'NONE', #915, #5671, #15247 ) ;
#4198 = DIRECTION ( 'NONE',  ( 1.000000000000000000, 0.000000000000000000, 0.000000000000000000 ) ) ;
#4199 = MANIFOLD_SOLID_BREP ( 'Fillet2', #630 ) ;
#4200 = CARTESIAN_POINT ( 'NONE',  ( 0.000000000000000000, 0.000000000000000000, -0.05905511811023622659 ) ) ;
#4201 = CARTESIAN_POINT ( 'NONE',  ( -0.4307978335858689278, -0.003937007874015747977, 0.4279391777402706820 ) ) ;
#4202 = AXIS2_PLACEMENT_3D ( 'NONE', #7048, #4393, #4543 ) ;
#4203 = DIRECTION ( 'NONE',  ( -1.000000000000000000, -8.673617379884013384E-15, 0.000000000000000000 ) ) ;
#4204 = FILL_AREA_STYLE ('',( #14950 ) ) ;
#4205 = ORIENTED_EDGE ( 'NONE', *, *, #14574, .F. ) ;
#4206 = ORIENTED_EDGE ( 'NONE', *, *, #14724, .F. ) ;
#4207 = AXIS2_PLACEMENT_3D ( 'NONE', #4232, #9020, #10332 ) ;
#4208 = EDGE_LOOP ( 'NONE', ( #7967, #9982, #7104 ) ) ;
#4209 = ORIENTED_EDGE ( 'NONE', *, *, #15043, .T. ) ;
#4210 = EDGE_LOOP ( 'NONE', ( #5386, #4920, #9552, #5144 ) ) ;
#4211 = AXIS2_PLACEMENT_3D ( 'NONE', #7409, #148, #9933 ) ;
#4212 = DIRECTION ( 'NONE',  ( 1.000000000000000000, 0.000000000000000000, 0.000000000000000000 ) ) ;
#4213 = DIRECTION ( 'NONE',  ( -0.4999999999999979461, -0.000000000000000000, -0.8660254037844398178 ) ) ;
#4214 = DIRECTION ( 'NONE',  ( 0.5000000000000004441, -0.000000000000000000, -0.8660254037844384856 ) ) ;
#4215 = LINE ( 'NONE', #538, #3187 ) ;
#4216 = DIRECTION ( 'NONE',  ( -1.000000000000000000, 0.000000000000000000, -0.000000000000000000 ) ) ;
#4217 = DIRECTION ( 'NONE',  ( -0.000000000000000000, -1.000000000000000000, -0.000000000000000000 ) ) ;
#4218 = DIRECTION ( 'NONE',  ( -1.000000000000000000, 0.000000000000000000, 0.000000000000000000 ) ) ;
#4219 = CARTESIAN_POINT ( 'NONE',  ( -0.06692913385815749128, -0.4881889763779528324, -0.2377126739438355507 ) ) ;
#4220 = CARTESIAN_POINT ( 'NONE',  ( -1.925369493808086974, -2.803727943723343774, -0.1746073045697247028 ) ) ;
#4221 = ORIENTED_EDGE ( 'NONE', *, *, #1008, .F. ) ;
#4222 = CARTESIAN_POINT ( 'NONE',  ( -0.5905511811023621549, 2.440944881889763884, -0.04724409448818898266 ) ) ;
#4223 = CARTESIAN_POINT ( 'NONE',  ( -1.588328939002293660, 0.1239872266390858180, 0.03937007874015745895 ) ) ;
#4224 = EDGE_LOOP ( 'NONE', ( #3303, #14565, #6370, #5715 ) ) ;
#4225 = ORIENTED_EDGE ( 'NONE', *, *, #5196, .F. ) ;
#4226 = ADVANCED_FACE ( 'NONE', ( #15318, #8563 ), #5254, .T. ) ;
#4227 = ORIENTED_EDGE ( 'NONE', *, *, #13243, .F. ) ;
#4228 = ADVANCED_FACE ( 'NONE', ( #6273, #13273 ), #4022, .F. ) ;
#4229 = EDGE_CURVE ( 'NONE', #6660, #6983, #2840, .T. ) ;
#4230 = DIRECTION ( 'NONE',  ( 0.000000000000000000, 0.000000000000000000, -1.000000000000000000 ) ) ;
#4231 = DIRECTION ( 'NONE',  ( 0.000000000000000000, 0.000000000000000000, 1.000000000000000000 ) ) ;
#4232 = CARTESIAN_POINT ( 'NONE',  ( 0.000000000000000000, 2.440944881889763884, 0.000000000000000000 ) ) ;
#4233 = DIRECTION ( 'NONE',  ( 2.168404344971007142E-16, 0.000000000000000000, -1.000000000000000000 ) ) ;
#4234 = VERTEX_POINT ( 'NONE', #7471 ) ;
#4235 = DIRECTION ( 'NONE',  ( 0.000000000000000000, 0.000000000000000000, 1.000000000000000000 ) ) ;
#4236 = CARTESIAN_POINT ( 'NONE',  ( 0.000000000000000000, 1.385826771653543510, 0.000000000000000000 ) ) ;
#4237 = DIRECTION ( 'NONE',  ( -0.000000000000000000, 0.000000000000000000, 1.000000000000000000 ) ) ;
#4238 = DIRECTION ( 'NONE',  ( -0.4999999999999975575, 0.000000000000000000, -0.8660254037844399289 ) ) ;
#4239 = EDGE_LOOP ( 'NONE', ( #12833, #1528, #12404, #10080 ) ) ;
#4240 =( NAMED_UNIT ( * ) PLANE_ANGLE_UNIT ( ) SI_UNIT ( $, .RADIAN. ) );
#4241 = ORIENTED_EDGE ( 'NONE', *, *, #9033, .T. ) ;
#4242 = EDGE_CURVE ( 'NONE', #11911, #15201, #11612, .T. ) ;
#4243 = ORIENTED_EDGE ( 'NONE', *, *, #4928, .F. ) ;
#4244 = EDGE_CURVE ( 'NONE', #3700, #12957, #1840, .T. ) ;
#4245 = DIRECTION ( 'NONE',  ( 0.000000000000000000, 1.000000000000000000, 0.000000000000000000 ) ) ;
#4246 = DIRECTION ( 'NONE',  ( 0.000000000000000000, 0.000000000000000000, -1.000000000000000000 ) ) ;
#4247 = EDGE_CURVE ( 'NONE', #4854, #9785, #2349, .T. ) ;
#4248 = CARTESIAN_POINT ( 'NONE',  ( 1.928577636452524610E-17, -0.4881889763779528324, -0.1574803149606299191 ) ) ;
#4249 = DIRECTION ( 'NONE',  ( -1.000000000000000000, 0.000000000000000000, 0.000000000000000000 ) ) ;
#4250 = PRODUCT_CONTEXT ( 'NONE', #8399, 'mechanical' ) ;
#4251 = EDGE_CURVE ( 'NONE', #11239, #4631, #13346, .T. ) ;
#4252 = CARTESIAN_POINT ( 'NONE',  ( 0.09061599198715353243, 0.000000000000000000, 0.007444810018878659542 ) ) ;
#4253 = ORIENTED_EDGE ( 'NONE', *, *, #7387, .F. ) ;
#4254 = DIRECTION ( 'NONE',  ( -0.000000000000000000, -1.000000000000000000, -0.000000000000000000 ) ) ;
#4255 = DIRECTION ( 'NONE',  ( 0.5984233124757297739, 0.8011800915434527104, 2.779651826571349572E-15 ) ) ;
#4256 = CARTESIAN_POINT ( 'NONE',  ( 0.3314531923919106227, -0.2952755905511811330, 0.2641016316388982710 ) ) ;
#4257 = CARTESIAN_POINT ( 'NONE',  ( 1.181102362204724310, 4.044111181948214319E-16, 0.02952755905511811330 ) ) ;
#4258 = ORIENTED_EDGE ( 'NONE', *, *, #12409, .F. ) ;
#4259 = ORIENTED_EDGE ( 'NONE', *, *, #12386, .T. ) ;
#4260 = ORIENTED_EDGE ( 'NONE', *, *, #260, .F. ) ;
#4261 = ORIENTED_EDGE ( 'NONE', *, *, #14413, .T. ) ;
#4262 = CARTESIAN_POINT ( 'NONE',  ( -0.1023622047242991467, -0.1023622047244094474, -0.5870514566507987197 ) ) ;
#4263 = CARTESIAN_POINT ( 'NONE',  ( -1.995574620099673124, -2.802153887077456940, 0.1558670272671928148 ) ) ;
#4264 = DIRECTION ( 'NONE',  ( 0.000000000000000000, 0.000000000000000000, 1.000000000000000000 ) ) ;
#4265 = EDGE_CURVE ( 'NONE', #15416, #6036, #6690, .T. ) ;
#4266 = DIRECTION ( 'NONE',  ( 0.4999999999999983347, -0.000000000000000000, 0.8660254037844397068 ) ) ;
#4267 =( BOUNDED_SURFACE ( )  B_SPLINE_SURFACE ( 3, 2, ( 
 ( #4539, #9321, #14098 ),
 ( #3374, #12933, #2203 ),
 ( #6976, #11767, #13792 ),
 ( #3057, #7828, #12622 ),
 ( #4935, #5778, #2341 ),
 ( #2501, #14264, #2431 ) ),
 .UNSPECIFIED., .F., .F., .T. ) 
 B_SPLINE_SURFACE_WITH_KNOTS ( ( 4, 2, 4 ),
 ( 3, 3 ),
 ( -3.623019766860193592E-05, 0.0007449614524473009095, 0.001526153102563203735 ),
 ( 0.000000000000000000, 1.000000000000000000 ),
 .UNSPECIFIED. ) 
 GEOMETRIC_REPRESENTATION_ITEM ( )  RATIONAL_B_SPLINE_SURFACE ( (
 ( 1.000000000000000000, 1.000000000000000000, 1.000000000000000000),
 ( 1.000000000000000000, 1.000000656565404711, 1.000000000000000000),
 ( 1.000000000000000000, 0.9999739034942860538, 1.000000000000000000),
 ( 1.000000000000000000, 0.9999216474068313154, 1.000000000000000000),
 ( 1.000000000000000000, 0.9998986130898210867, 1.000000000000000000),
 ( 1.000000000000000000, 0.9998995914418474795, 1.000000000000000000) ) ) 
 REPRESENTATION_ITEM ( '' )  SURFACE ( )  );
#4268 = CARTESIAN_POINT ( 'NONE',  ( -1.955396564714622976, -2.907528569965089460, -0.1152285774067266372 ) ) ;
#4269 = DIRECTION ( 'NONE',  ( 0.000000000000000000, 0.000000000000000000, -1.000000000000000000 ) ) ;
#4270 = DIRECTION ( 'NONE',  ( -0.000000000000000000, 0.000000000000000000, 1.000000000000000000 ) ) ;
#4271 = EDGE_CURVE ( 'NONE', #1905, #11305, #11095, .T. ) ;
#4272 = DIRECTION ( 'NONE',  ( -0.3235667741753706084, 0.9383274424966834282, 0.1218447918762960436 ) ) ;
#4273 = CARTESIAN_POINT ( 'NONE',  ( -2.080881322745466555, -1.632190302820504701, -0.1033464566929128137 ) ) ;
#4274 = ORIENTED_EDGE ( 'NONE', *, *, #3092, .T. ) ;
#4275 = EDGE_LOOP ( 'NONE', ( #5762, #5595, #14067, #12885 ) ) ;
#4276 = EDGE_LOOP ( 'NONE', ( #12752, #7038, #9150 ) ) ;
#4277 = ORIENTED_EDGE ( 'NONE', *, *, #3420, .F. ) ;
#4278 = CARTESIAN_POINT ( 'NONE',  ( 0.000000000000000000, 1.425196850393700920, -0.6692913385826770867 ) ) ;
#4279 = LINE ( 'NONE', #9067, #15119 ) ;
#4280 = CARTESIAN_POINT ( 'NONE',  ( 0.2661821753648509481, -0.1023622047244094474, 0.03548265769547701703 ) ) ;
#4281 = CARTESIAN_POINT ( 'NONE',  ( 0.05905511811023622659, 1.338626482899105241, -0.5946706712680680518 ) ) ;
#4282 = CARTESIAN_POINT ( 'NONE',  ( 0.000000000000000000, 0.5511811023622046335, 0.000000000000000000 ) ) ;
#4283 = DIRECTION ( 'NONE',  ( 0.000000000000000000, 1.000000000000000000, -0.000000000000000000 ) ) ;
#4284 = LINE ( 'NONE', #4366, #7966 ) ;
#4285 = CARTESIAN_POINT ( 'NONE',  ( -1.926829032957098509, -2.799642034967062543, -0.1538761875634443999 ) ) ;
#4286 = VERTEX_POINT ( 'NONE', #5030 ) ;
#4287 = CYLINDRICAL_SURFACE ( 'NONE', #7428, 0.03937007874015754916 ) ;
#4288 = EDGE_CURVE ( 'NONE', #15235, #10603, #13566, .T. ) ;
#4290 = EDGE_LOOP ( 'NONE', ( #11419, #2348, #10012, #14808 ) ) ;
#4289 =( REPRESENTATION_RELATIONSHIP ('NONE','NONE', #8904, #11075 ) REPRESENTATION_RELATIONSHIP_WITH_TRANSFORMATION ( #7290 )SHAPE_REPRESENTATION_RELATIONSHIP( ) );
#4291 = ORIENTED_EDGE ( 'NONE', *, *, #2805, .F. ) ;
#4292 = ORIENTED_EDGE ( 'NONE', *, *, #3481, .F. ) ;
#4293 = DIRECTION ( 'NONE',  ( 0.5000000000000004441, 0.000000000000000000, 0.8660254037844383745 ) ) ;
#4294 = CYLINDRICAL_SURFACE ( 'NONE', #1124, 0.003937007874015744507 ) ;
#4295 = CARTESIAN_POINT ( 'NONE',  ( -0.4841913566216235476, 1.043107366814280734, 0.3477389867607276752 ) ) ;
#4296 = CARTESIAN_POINT ( 'NONE',  ( 0.2393297813660762718, -0.4881889763779528324, 0.06089400679746261730 ) ) ;
#4297 = FACE_OUTER_BOUND ( 'NONE', #6486, .T. ) ;
#4298 = ORIENTED_EDGE ( 'NONE', *, *, #1265, .T. ) ;
#4299 = DIRECTION ( 'NONE',  ( -0.4999999999999986122, 0.000000000000000000, 0.8660254037844395958 ) ) ;
#4300 = CARTESIAN_POINT ( 'NONE',  ( -1.580259682937507515, 0.1018956540318727566, 0.1968503937007874127 ) ) ;
#4301 = CARTESIAN_POINT ( 'NONE',  ( 0.000000000000000000, 0.5905511811023621549, 0.000000000000000000 ) ) ;
#4302 = EDGE_CURVE ( 'NONE', #6217, #15003, #14832, .T. ) ;
#4303 = CYLINDRICAL_SURFACE ( 'NONE', #8344, 0.01968503937007877111 ) ;
#4304 = EDGE_LOOP ( 'NONE', ( #11415, #14431, #11497, #5051, #8034, #11069 ) ) ;
#4305 = CARTESIAN_POINT ( 'NONE',  ( -0.5084014747882513729, -0.003937007874015747977, 0.2935257283253980831 ) ) ;
#4306 = ORIENTED_EDGE ( 'NONE', *, *, #9756, .T. ) ;
#4307 = EDGE_CURVE ( 'NONE', #9168, #11283, #8602, .T. ) ;
#4308 = ORIENTED_EDGE ( 'NONE', *, *, #2335, .T. ) ;
#4309 = ORIENTED_EDGE ( 'NONE', *, *, #9534, .F. ) ;
#4310 = CARTESIAN_POINT ( 'NONE',  ( 0.000000000000000000, 1.409448818897637956, -0.5511811023622046335 ) ) ;
#4311 = DIRECTION ( 'NONE',  ( -0.000000000000000000, 1.000000000000000000, 0.000000000000000000 ) ) ;
#4312 = CYLINDRICAL_SURFACE ( 'NONE', #5340, 0.003937007874015758385 ) ;
#4313 = FACE_OUTER_BOUND ( 'NONE', #12269, .T. ) ;
#4314 = ITEM_DEFINED_TRANSFORMATION ( 'NONE', 'NONE', #10863,  #11481 ) ;
#4315 = DIRECTION ( 'NONE',  ( 0.000000000000000000, 0.000000000000000000, 1.000000000000000000 ) ) ;
#4316 = CIRCLE ( 'NONE', #5810, 0.003937007874015749712 ) ;
#4317 = DIRECTION ( 'NONE',  ( 0.4005670834070333974, 0.9162674345903507600, -5.558984986317924027E-15 ) ) ;
#4318 = VERTEX_POINT ( 'NONE', #13725 ) ;
#4319 = CARTESIAN_POINT ( 'NONE',  ( 0.03346456692910664693, -0.4921259842519685179, -0.05796233017450188457 ) ) ;
#4320 = AXIS2_PLACEMENT_3D ( 'NONE', #2259, #11906, #13146 ) ;
#4321 = EDGE_CURVE ( 'NONE', #25, #7594, #12613, .T. ) ;
#4322 = AXIS2_PLACEMENT_3D ( 'NONE', #10962, #9725, #9868 ) ;
#4323 = DIRECTION ( 'NONE',  ( 0.000000000000000000, -0.000000000000000000, -1.000000000000000000 ) ) ;
#4324 = EDGE_CURVE ( 'NONE', #11956, #3678, #15111, .T. ) ;
#4325 = CARTESIAN_POINT ( 'NONE',  ( 8.148240514011916814E-17, 1.614173228346457156, -0.6614173228346456046 ) ) ;
#4326 = VERTEX_POINT ( 'NONE', #8949 ) ;
#4327 = ORIENTED_EDGE ( 'NONE', *, *, #12395, .T. ) ;
#4328 = ADVANCED_FACE ( 'NONE', ( #12387 ), #1348, .F. ) ;
#4329 = CARTESIAN_POINT ( 'NONE',  ( 0.000000000000000000, 0.5905511811023621549, 0.000000000000000000 ) ) ;
#4331 = EDGE_LOOP ( 'NONE', ( #185, #2308, #7908, #363 ) ) ;
#4330 = CIRCLE ( 'NONE', #8328, 0.003937007874015754916 ) ;
#4332 = AXIS2_PLACEMENT_3D ( 'NONE', #211, #12099, #12261 ) ;
#4333 = VERTEX_POINT ( 'NONE', #2674 ) ;
#4334 = AXIS2_PLACEMENT_3D ( 'NONE', #9815, #8633, #14518 ) ;
#4335 = CARTESIAN_POINT ( 'NONE',  ( -0.4749369078591176296, -0.1023622047244094474, 0.3514880584999472424 ) ) ;
#4336 = CARTESIAN_POINT ( 'NONE',  ( -1.980019913028319367, -2.844306626094838641, 0.1438463815136533930 ) ) ;
#4337 = SHAPE_REPRESENTATION_RELATIONSHIP ( 'NONE' , 'NONE' ,  #12705, #8362 ) ;
#4338 = DIMENSIONAL_EXPONENTS ( 1.000000000000000000, 0.000000000000000000, 0.000000000000000000, 0.000000000000000000, 0.000000000000000000, 0.000000000000000000, 0.000000000000000000 ) ;
#4339 = DIRECTION ( 'NONE',  ( -0.8660254037844433705, 0.000000000000000000, -0.4999999999999918954 ) ) ;
#4340 = CARTESIAN_POINT ( 'NONE',  ( 0.000000000000000000, 1.614173228346457156, 0.000000000000000000 ) ) ;
#4341 = TOROIDAL_SURFACE ( 'NONE', #1601, 0.007874015748031495954, 0.003937007874015747977 ) ;
#4342 = AXIS2_PLACEMENT_3D ( 'NONE', #7077, #5904, #4799 ) ;
#4343 = PLANE ( 'NONE',  #7391 ) ;
#4344 = EDGE_CURVE ( 'NONE', #14791, #10242, #7364, .T. ) ;
#4345 = AXIS2_PLACEMENT_3D ( 'NONE', #6130, #7587, #1660 ) ;
#4346 = CARTESIAN_POINT ( 'NONE',  ( 0.4815353412745266848, 1.041793866378536437, 0.3474236500605469291 ) ) ;
#4347 = CARTESIAN_POINT ( 'NONE',  ( -2.087493674894419282, -2.010784418770093840, -0.1111536532825547208 ) ) ;
#4348 = CIRCLE ( 'NONE', #616, 0.003937007874015758385 ) ;
#4349 = VECTOR ( 'NONE', #4020, 39.37007874015748143 ) ;
#4350 = ORIENTED_EDGE ( 'NONE', *, *, #14152, .F. ) ;
#4351 = EDGE_CURVE ( 'NONE', #4716, #6519, #10609, .T. ) ;
#4352 = EDGE_LOOP ( 'NONE', ( #7071, #8143, #4042, #14194 ) ) ;
#4353 = EDGE_CURVE ( 'NONE', #8715, #5216, #1431, .T. ) ;
#4354 = ORIENTED_EDGE ( 'NONE', *, *, #5667, .T. ) ;
#4355 = ORIENTED_EDGE ( 'NONE', *, *, #12900, .F. ) ;
#4356 = AXIS2_PLACEMENT_3D ( 'NONE', #9070, #6628, #4216 ) ;
#4357 = CIRCLE ( 'NONE', #8412, 0.01968503937007873988 ) ;
#4358 = VECTOR ( 'NONE', #9219, 39.37007874015748143 ) ;
#4359 = EDGE_CURVE ( 'NONE', #113, #7319, #14901, .T. ) ;
#4360 = CARTESIAN_POINT ( 'NONE',  ( 1.181102362204724310, 4.044111181948214319E-16, 0.02952755905511811330 ) ) ;
#4361 = CARTESIAN_POINT ( 'NONE',  ( -1.315994971760645248E-15, -0.003937007874015747977, 0.4279391777402719588 ) ) ;
#4362 = CARTESIAN_POINT ( 'NONE',  ( -0.1771653543307086243, -0.02638708502139245488, 0.03937007874015747977 ) ) ;
#4363 = AXIS2_PLACEMENT_3D ( 'NONE', #1520, #3726, #8650 ) ;
#4364 = CARTESIAN_POINT ( 'NONE',  ( -1.181102362204724310, -0.1240157480314959815, -0.02952755905511811330 ) ) ;
#4365 = CARTESIAN_POINT ( 'NONE',  ( -1.431036756819011213, -0.02829858486107876200, 0.1968503937007874127 ) ) ;
#4366 = CARTESIAN_POINT ( 'NONE',  ( -0.000000000000000000, -0.09842519685039370636, 0.1689446513984334541 ) ) ;
#4367 = DIRECTION ( 'NONE',  ( 5.457303053353514501E-25, 1.000000000000000000, -6.049848122469114742E-13 ) ) ;
#4368 = ORIENTED_EDGE ( 'NONE', *, *, #14866, .T. ) ;
#4369 = DIRECTION ( 'NONE',  ( -1.000000000000000000, 0.000000000000000000, 0.000000000000000000 ) ) ;
#4370 = CARTESIAN_POINT ( 'NONE',  ( -0.3512416941306060192, -0.2952755905511811330, 0.3164411144501575457 ) ) ;
#4371 = AXIS2_PLACEMENT_3D ( 'NONE', #9439, #8013, #9269 ) ;
#4372 = AXIS2_PLACEMENT_3D ( 'NONE', #8090, #10452, #15231 ) ;
#4373 = AXIS2_PLACEMENT_3D ( 'NONE', #1147, #14061, #13113 ) ;
#4374 = ORIENTED_EDGE ( 'NONE', *, *, #8690, .F. ) ;
#4375 = EDGE_LOOP ( 'NONE', ( #14133, #1965, #9782, #3817, #6684, #3361 ) ) ;
#4376 = EDGE_CURVE ( 'NONE', #10028, #9980, #4005, .T. ) ;
#4377 = AXIS2_PLACEMENT_3D ( 'NONE', #13237, #11026, #3685 ) ;
#4378 = ORIENTED_EDGE ( 'NONE', *, *, #10000, .F. ) ;
#4379 = CARTESIAN_POINT ( 'NONE',  ( -0.5398975377803494347, -0.1023622047244094474, 0.2389729469846940679 ) ) ;
#4380 = EDGE_CURVE ( 'NONE', #5718, #12092, #14108, .T. ) ;
#4381 = CIRCLE ( 'NONE', #3885, 0.1240157480314959260 ) ;
#4382 = AXIS2_PLACEMENT_3D ( 'NONE', #4370, #11578, #5090 ) ;
#4383 = AXIS2_PLACEMENT_3D ( 'NONE', #10729, #10, #4837 ) ;
#4384 = CARTESIAN_POINT ( 'NONE',  ( -0.4591888763630546655, -0.09842519685039370636, 0.3787644491703233141 ) ) ;
#4385 = CARTESIAN_POINT ( 'NONE',  ( -1.931900750301128511, -2.930638880368575006, -0.08039528988028955825 ) ) ;
#4386 = DIRECTION ( 'NONE',  ( 1.000000000000000000, 0.000000000000000000, 0.000000000000000000 ) ) ;
#4387 = DIRECTION ( 'NONE',  ( -0.000000000000000000, -1.000000000000000000, -0.000000000000000000 ) ) ;
#4388 = VECTOR ( 'NONE', #8501, 39.37007874015747433 ) ;
#4389 = CARTESIAN_POINT ( 'NONE',  ( 0.06299212598430634080, -0.1023622047244094474, -0.2377126739437405434 ) ) ;
#4390 = EDGE_LOOP ( 'NONE', ( #13169, #6390, #8706, #3766 ) ) ;
#4391 = CARTESIAN_POINT ( 'NONE',  ( -1.431036756819011213, -0.02829858486107871343, 0.07874015748031495954 ) ) ;
#4392 = LINE ( 'NONE', #13732, #11352 ) ;
#4393 = DIRECTION ( 'NONE',  ( 0.000000000000000000, -1.000000000000000000, 0.000000000000000000 ) ) ;
#4394 = DIRECTION ( 'NONE',  ( 0.000000000000000000, 0.000000000000000000, -1.000000000000000000 ) ) ;
#4395 = VERTEX_POINT ( 'NONE', #14669 ) ;
#4396 = DIRECTION ( 'NONE',  ( 0.000000000000000000, 0.000000000000000000, -1.000000000000000000 ) ) ;
#4397 = AXIS2_PLACEMENT_3D ( 'NONE', #12489, #6504, #5249 ) ;
#4398 = CIRCLE ( 'NONE', #11150, 0.04330708661417326938 ) ;
#4399 = CIRCLE ( 'NONE', #15418, 0.003937007874015749712 ) ;
#4400 = ORIENTED_EDGE ( 'NONE', *, *, #1125, .F. ) ;
#4401 = VERTEX_POINT ( 'NONE', #7683 ) ;
#4402 = AXIS2_PLACEMENT_3D ( 'NONE', #14213, #11787, #3482 ) ;
#4403 = ORIENTED_EDGE ( 'NONE', *, *, #12961, .F. ) ;
#4404 = DIRECTION ( 'NONE',  ( 0.000000000000000000, -1.000000000000000000, -0.000000000000000000 ) ) ;
#4405 = CARTESIAN_POINT ( 'NONE',  ( 0.5418660417173575272, -0.4881889763779528324, 0.2355633981508976349 ) ) ;
#4406 = CARTESIAN_POINT ( 'NONE',  ( -0.007954450877559391536, 0.1525563742224383124, -0.01590295032065047048 ) ) ;
#4407 = FACE_OUTER_BOUND ( 'NONE', #4148, .T. ) ;
#4408 = ITEM_DEFINED_TRANSFORMATION ( 'NONE', 'NONE', #9626,  #11481 ) ;
#4409 = CARTESIAN_POINT ( 'NONE',  ( 5.544660704801008561E-18, 0.05905511811023623353, -0.04527559055118110520 ) ) ;
#4410 = CIRCLE ( 'NONE', #5902, 0.003937007874015758385 ) ;
#4411 = CARTESIAN_POINT ( 'NONE',  ( 0.06604848736013263499, 0.000000000000000000, -0.5868460571724355423 ) ) ;
#4412 = EDGE_LOOP ( 'NONE', ( #12693, #11256 ) ) ;
#4413 = CARTESIAN_POINT ( 'NONE',  ( 0.000000000000000000, 2.401574803149606918, 0.000000000000000000 ) ) ;
#4414 = FACE_OUTER_BOUND ( 'NONE', #3315, .T. ) ;
#4415 = CIRCLE ( 'NONE', #3178, 0.5905511811023621549 ) ;
#4416 = PLANE ( 'NONE',  #11708 ) ;
#4417 = DIRECTION ( 'NONE',  ( 0.5000000000000004441, 0.000000000000000000, -0.8660254037844383745 ) ) ;
#4418 = ORIENTED_EDGE ( 'NONE', *, *, #3570, .T. ) ;
#4419 = ORIENTED_EDGE ( 'NONE', *, *, #10000, .T. ) ;
#4420 = PLANE ( 'NONE',  #684 ) ;
#4421 = ORIENTED_EDGE ( 'NONE', *, *, #8396, .F. ) ;
#4422 = CIRCLE ( 'NONE', #1679, 0.7086614173228346081 ) ;
#4423 = ORIENTED_EDGE ( 'NONE', *, *, #3199, .T. ) ;
#4424 = EDGE_CURVE ( 'NONE', #8620, #1922, #3848, .T. ) ;
#4425 = AXIS2_PLACEMENT_3D ( 'NONE', #4161, #12624, #2817 ) ;
#4426 = ADVANCED_FACE ( 'NONE', ( #10977 ), #1502, .T. ) ;
#4427 = CARTESIAN_POINT ( 'NONE',  ( 1.141732283464566677, 4.044111181948214319E-16, 0.02952755905511811330 ) ) ;
#4428 = CARTESIAN_POINT ( 'NONE',  ( -0.7455328141524873997, 1.190944881889763884, 0.3622425942647021779 ) ) ;
#4429 = AXIS2_PLACEMENT_3D ( 'NONE', #6508, #12730, #13810 ) ;
#4430 = FACE_OUTER_BOUND ( 'NONE', #7180, .T. ) ;
#4431 = CARTESIAN_POINT ( 'NONE',  ( -1.576201932089153157, 0.1075912864655425849, -0.06349180857188843619 ) ) ;
#4432 = ADVANCED_FACE ( 'NONE', ( #12473 ), #11279, .T. ) ;
#4433 = CIRCLE ( 'NONE', #13198, 0.1574803149606299191 ) ;
#4434 = CARTESIAN_POINT ( 'NONE',  ( -0.3944453183761345572, -0.2952755905511811330, 0.1549960689574421957 ) ) ;
#4435 = VECTOR ( 'NONE', #4135, 39.37007874015748143 ) ;
#4436 = CARTESIAN_POINT ( 'NONE',  ( -1.181102362204724310, 0.000000000000000000, -0.02559055118110236185 ) ) ;
#4437 = CARTESIAN_POINT ( 'NONE',  ( -2.080881322745466999, -1.632190302820504479, -0.08366141732283406685 ) ) ;
#4438 = CIRCLE ( 'NONE', #936, 0.5826771653543306728 ) ;
#4439 = ORIENTED_EDGE ( 'NONE', *, *, #8460, .T. ) ;
#4440 = ORIENTED_EDGE ( 'NONE', *, *, #6473, .F. ) ;
#4441 = AXIS2_PLACEMENT_3D ( 'NONE', #7227, #3543, #8081 ) ;
#4442 = ORIENTED_EDGE ( 'NONE', *, *, #12186, .F. ) ;
#4443 = ORIENTED_EDGE ( 'NONE', *, *, #4904, .F. ) ;
#4444 = EDGE_CURVE ( 'NONE', #11529, #13463, #11040, .T. ) ;
#4445 = AXIS2_PLACEMENT_3D ( 'NONE', #6692, #13685, #8987 ) ;
#4446 = EDGE_CURVE ( 'NONE', #14049, #7994, #12380, .T. ) ;
#4447 = CARTESIAN_POINT ( 'NONE',  ( -1.584115185264708403, 0.1296286773226378863, -0.03937007874015747977 ) ) ;
#4448 = DIRECTION ( 'NONE',  ( -1.000000000000000000, 0.000000000000000000, -3.075191616504340279E-15 ) ) ;
#4449 = AXIS2_PLACEMENT_3D ( 'NONE', #5658, #13982, #2147 ) ;
#4450 = DIRECTION ( 'NONE',  ( -1.000000000000000000, 0.000000000000000000, 0.000000000000000000 ) ) ;
#4451 = CARTESIAN_POINT ( 'NONE',  ( 0.05905511811023622659, 1.338582677165354395, -0.5955041639236611228 ) ) ;
#4452 = EDGE_CURVE ( 'NONE', #15344, #14180, #6347, .T. ) ;
#4453 = DIRECTION ( 'NONE',  ( -0.000000000000000000, -1.000000000000000000, -0.000000000000000000 ) ) ;
#4454 = CARTESIAN_POINT ( 'NONE',  ( 5.303588500244448531E-18, 0.07874015748031495954, -0.04330708661417326938 ) ) ;
#4455 = CARTESIAN_POINT ( 'NONE',  ( -1.937736976485135987, -2.834264970500691039, -0.1664422342211422379 ) ) ;
#4456 = VERTEX_POINT ( 'NONE', #12307 ) ;
#4457 = DIRECTION ( 'NONE',  ( -1.000000000000000000, 2.168404344971007142E-16, 0.000000000000000000 ) ) ;
#4458 = CARTESIAN_POINT ( 'NONE',  ( -1.181102362204724310, 0.000000000000000000, 0.02952755905511811330 ) ) ;
#4459 = AXIS2_PLACEMENT_3D ( 'NONE', #6730, #1971, #11519 ) ;
#4460 = EDGE_LOOP ( 'NONE', ( #1995, #10417, #7267, #8920 ) ) ;
#4461 = ORIENTED_EDGE ( 'NONE', *, *, #11912, .F. ) ;
#4462 = CIRCLE ( 'NONE', #12738, 0.01968503937007871213 ) ;
#4463 = ORIENTED_EDGE ( 'NONE', *, *, #7029, .F. ) ;
#4464 = FACE_OUTER_BOUND ( 'NONE', #9313, .T. ) ;
#4465 = CIRCLE ( 'NONE', #13981, 0.007874015748031516770 ) ;
#4466 = CYLINDRICAL_SURFACE ( 'NONE', #15377, 0.003937007874015721089 ) ;
#4467 = CARTESIAN_POINT ( 'NONE',  ( -0.2681506793016945611, -0.1023622047244094474, 0.03207310886158500768 ) ) ;
#4468 = ADVANCED_FACE ( 'NONE', ( #1565, #6324 ), #11124, .T. ) ;
#4469 = FACE_OUTER_BOUND ( 'NONE', #3172, .T. ) ;
#4470 = DIRECTION ( 'NONE',  ( 0.000000000000000000, 0.000000000000000000, 1.000000000000000000 ) ) ;
#4471 = ORIENTED_EDGE ( 'NONE', *, *, #8488, .T. ) ;
#4472 = CARTESIAN_POINT ( 'NONE',  ( -1.293236445124221312, 0.1355266887446167634, 0.05905511811023622659 ) ) ;
#4473 = DIRECTION ( 'NONE',  ( 1.224646799147343593E-16, 0.000000000000000000, -1.000000000000000000 ) ) ;
#4474 = CARTESIAN_POINT ( 'NONE',  ( -0.1763376553817701808, -0.1023622047244094474, 0.1699995694788709877 ) ) ;
#4475 = CARTESIAN_POINT ( 'NONE',  ( -1.181342415325336237, 0.3435647566446753398, 0.04457061940634219482 ) ) ;
#4476 = ORIENTED_EDGE ( 'NONE', *, *, #14152, .T. ) ;
#4477 = ADVANCED_FACE ( 'NONE', ( #9017 ), #2606, .T. ) ;
#4478 = FACE_OUTER_BOUND ( 'NONE', #12423, .T. ) ;
#4479 = EDGE_LOOP ( 'NONE', ( #1020, #4989, #3962, #12878, #6811, #7941, #13011, #15052, #2569, #15036 ) ) ;
#4480 = EDGE_LOOP ( 'NONE', ( #12762, #13832, #11259, #10412 ) ) ;
#4481 = ORIENTED_EDGE ( 'NONE', *, *, #13680, .F. ) ;
#4482 = CARTESIAN_POINT ( 'NONE',  ( -0.2353927734918962178, -0.1023622047244094474, 0.06771310446496157931 ) ) ;
#4483 = CARTESIAN_POINT ( 'NONE',  ( 0.1724006475077543565, -0.4881889763779528324, 0.1768186671464649640 ) ) ;
#4484 = CARTESIAN_POINT ( 'NONE',  ( 0.5894146648244296127, -0.003937007874015747977, 0.1610807828475372405 ) ) ;
#4485 = FACE_BOUND ( 'NONE', #2557, .T. ) ;
#4486 = ITEM_DEFINED_TRANSFORMATION ( 'NONE', 'NONE', #11370,  #11481 ) ;
#4487 = CARTESIAN_POINT ( 'NONE',  ( -1.181342415325333350, 0.3435647566446739520, -0.03937007874015747977 ) ) ;
#4488 = FACE_OUTER_BOUND ( 'NONE', #9537, .T. ) ;
#4489 = EDGE_LOOP ( 'NONE', ( #7632, #1425, #1319, #7884 ) ) ;
#4490 = DIRECTION ( 'NONE',  ( -0.000000000000000000, 1.000000000000000000, 0.000000000000000000 ) ) ;
#4491 = DIRECTION ( 'NONE',  ( -0.000000000000000000, 1.000000000000000000, 0.000000000000000000 ) ) ;
#4492 = DIRECTION ( 'NONE',  ( 0.000000000000000000, 2.212657494868377674E-16, 1.000000000000000000 ) ) ;
#4493 =( NAMED_UNIT ( * ) SI_UNIT ( $, .STERADIAN. ) SOLID_ANGLE_UNIT ( ) );
#4494 = ORIENTED_EDGE ( 'NONE', *, *, #6875, .T. ) ;
#4495 = ORIENTED_EDGE ( 'NONE', *, *, #4050, .T. ) ;
#4496 = DIRECTION ( 'NONE',  ( 0.8660254037844368202, 0.000000000000000000, -0.5000000000000032196 ) ) ;
#4497 = VERTEX_POINT ( 'NONE', #5705 ) ;
#4498 = EDGE_LOOP ( 'NONE', ( #7072, #14000, #495, #9334 ) ) ;
#4499 = VERTEX_POINT ( 'NONE', #13949 ) ;
#4500 = FACE_OUTER_BOUND ( 'NONE', #2033, .T. ) ;
#4501 = FACE_OUTER_BOUND ( 'NONE', #12134, .T. ) ;
#4502 = CARTESIAN_POINT ( 'NONE',  ( -0.6864776960422505070, 1.190944881889763884, 0.4645290592786119332 ) ) ;
#4503 = CARTESIAN_POINT ( 'NONE',  ( 0.000000000000000000, 0.000000000000000000, 0.000000000000000000 ) ) ;
#4504 = FACE_OUTER_BOUND ( 'NONE', #7090, .T. ) ;
#4505 = CARTESIAN_POINT ( 'NONE',  ( 0.4783464566929142014, -0.1023622047244094474, 0.3534565624369548908 ) ) ;
#4506 = CYLINDRICAL_SURFACE ( 'NONE', #14381, 0.03937007874015747977 ) ;
#4507 = ADVANCED_FACE ( 'NONE', ( #2029 ), #12617, .F. ) ;
#4508 = CARTESIAN_POINT ( 'NONE',  ( 0.4307978335858662633, -0.003937007874015747977, 0.4279391777402732910 ) ) ;
#4509 = PRESENTATION_STYLE_ASSIGNMENT (( #15251 ) ) ;
#4510 = EDGE_CURVE ( 'NONE', #8715, #5518, #5102, .T. ) ;
#4511 = ORIENTED_EDGE ( 'NONE', *, *, #235, .F. ) ;
#4512 = ORIENTED_EDGE ( 'NONE', *, *, #1184, .F. ) ;
#4513 = VERTEX_POINT ( 'NONE', #3053 ) ;
#4514 = ORIENTED_EDGE ( 'NONE', *, *, #5004, .T. ) ;
#4515 = EDGE_CURVE ( 'NONE', #2422, #6453, #5604, .T. ) ;
#4516 = DIRECTION ( 'NONE',  ( -0.000000000000000000, -0.000000000000000000, 1.000000000000000000 ) ) ;
#4517 = DIRECTION ( 'NONE',  ( 0.000000000000000000, -1.000000000000000000, 0.000000000000000000 ) ) ;
#4518 = LINE ( 'NONE', #9299, #9862 ) ;
#4519 = FACE_OUTER_BOUND ( 'NONE', #4479, .T. ) ;
#4520 = DIRECTION ( 'NONE',  ( -1.000000000000000000, 0.000000000000000000, 0.000000000000000000 ) ) ;
#4521 = DIRECTION ( 'NONE',  ( 0.000000000000000000, 0.000000000000000000, -1.000000000000000000 ) ) ;
#4522 = CARTESIAN_POINT ( 'NONE',  ( -1.181102362204724310, 0.000000000000000000, 0.02559055118110236185 ) ) ;
#4523 = CARTESIAN_POINT ( 'NONE',  ( -1.956731389022586809, -2.774113956945879700, -0.1775764214674195041 ) ) ;
#4524 = VERTEX_POINT ( 'NONE', #11681 ) ;
#4525 = DIRECTION ( 'NONE',  ( 0.000000000000000000, -1.000000000000000000, 0.000000000000000000 ) ) ;
#4526 = EDGE_CURVE ( 'NONE', #4567, #3617, #11363, .T. ) ;
#4527 = CARTESIAN_POINT ( 'NONE',  ( -0.01725179686542488086, 0.07136070614489399555, 0.07758808519268840798 ) ) ;
#4528 = ADVANCED_FACE ( 'NONE', ( #3138 ), #4294, .T. ) ;
#4529 = ADVANCED_FACE ( 'NONE', ( #10263 ), #3285, .F. ) ;
#4530 = VERTEX_POINT ( 'NONE', #7990 ) ;
#4531 = ORIENTED_EDGE ( 'NONE', *, *, #11806, .T. ) ;
#4532 = EDGE_CURVE ( 'NONE', #8791, #15270, #3115, .T. ) ;
#4533 = ORIENTED_EDGE ( 'NONE', *, *, #10975, .F. ) ;
#4534 = DIRECTION ( 'NONE',  ( 1.000000000000000000, 0.000000000000000000, 0.000000000000000000 ) ) ;
#4535 = CARTESIAN_POINT ( 'NONE',  ( -0.05905511811023622659, 1.190944881889763884, -0.8661417322834648047 ) ) ;
#4536 = CARTESIAN_POINT ( 'NONE',  ( -1.960310522231513364, -2.849326065546125886, 0.1599618923947356830 ) ) ;
#4537 = CARTESIAN_POINT ( 'NONE',  ( 0.06692913385832212347, -0.1023622047244094474, -0.5909884645248143498 ) ) ;
#4538 = CARTESIAN_POINT ( 'NONE',  ( 0.1743691514447621993, -0.4921259842519685179, 0.1734091183126679481 ) ) ;
#4539 = CARTESIAN_POINT ( 'NONE',  ( -1.190198933766848155, 0.3259758027579587325, -0.05905511811023622659 ) ) ;
#4540 = VERTEX_POINT ( 'NONE', #5539 ) ;
#4541 = CARTESIAN_POINT ( 'NONE',  ( -0.5871416322685659717, -0.09448818897637796532, 0.1571437749735178357 ) ) ;
#4542 = CARTESIAN_POINT ( 'NONE',  ( -0.05905511811023622659, 1.338877451511696792, -0.5922897223582481718 ) ) ;
#4543 = DIRECTION ( 'NONE',  ( 0.000000000000000000, -0.000000000000000000, -1.000000000000000000 ) ) ;
#4544 = ADVANCED_FACE ( 'NONE', ( #10424 ), #4466, .T. ) ;
#4545 = LINE ( 'NONE', #4712, #14845 ) ;
#4546 = ORIENTED_EDGE ( 'NONE', *, *, #5612, .T. ) ;
#4547 = FACE_OUTER_BOUND ( 'NONE', #14936, .T. ) ;
#4548 = VERTEX_POINT ( 'NONE', #4535 ) ;
#4549 = ADVANCED_FACE ( 'NONE', ( #10330 ), #1618, .T. ) ;
#4550 = ORIENTED_EDGE ( 'NONE', *, *, #5058, .F. ) ;
#4551 = EDGE_LOOP ( 'NONE', ( #7817, #6345, #4531, #9521 ) ) ;
#4552 = ORIENTED_EDGE ( 'NONE', *, *, #3176, .T. ) ;
#4553 = CARTESIAN_POINT ( 'NONE',  ( 0.000000000000000000, 1.614173228346457156, 0.000000000000000000 ) ) ;
#4554 = DIRECTION ( 'NONE',  ( -0.000000000000000000, -0.000000000000000000, -1.000000000000000000 ) ) ;
#4555 = ADVANCED_FACE ( 'NONE', ( #6727 ), #7913, .T. ) ;
#4556 = CARTESIAN_POINT ( 'NONE',  ( -0.5379290338433415641, -0.09448818897637796532, 0.2423824958184910838 ) ) ;
#4557 = CARTESIAN_POINT ( 'NONE',  ( -0.05905511811023622659, 1.043263280880422528, -0.5946706712680680518 ) ) ;
#4558 = DIRECTION ( 'NONE',  ( -0.000000000000000000, -0.000000000000000000, -1.000000000000000000 ) ) ;
#4559 = DIRECTION ( 'NONE',  ( -0.000000000000000000, -1.000000000000000000, -0.000000000000000000 ) ) ;
#4560 = ORIENTED_EDGE ( 'NONE', *, *, #5076, .F. ) ;
#4561 = FACE_OUTER_BOUND ( 'NONE', #8405, .T. ) ;
#4562 = CARTESIAN_POINT ( 'NONE',  ( -2.010991777528384095, -2.758467574604078543, -0.1561691687464109024 ) ) ;
#4563 = CARTESIAN_POINT ( 'NONE',  ( 0.000000000000000000, -0.1023622047244094474, -0.1614173228346456879 ) ) ;
#4564 = CIRCLE ( 'NONE', #3052, 0.003937007874015724558 ) ;
#4565 = DIRECTION ( 'NONE',  ( 0.5000000000000005551, 0.000000000000000000, -0.8660254037844384856 ) ) ;
#4566 = ORIENTED_EDGE ( 'NONE', *, *, #12977, .F. ) ;
#4567 = VERTEX_POINT ( 'NONE', #12771 ) ;
#4568 = DIRECTION ( 'NONE',  ( 0.4999999999999979461, -0.000000000000000000, 0.8660254037844398178 ) ) ;
#4569 = ORIENTED_EDGE ( 'NONE', *, *, #13482, .T. ) ;
#4570 = VERTEX_POINT ( 'NONE', #9317 ) ;
#4571 = ORIENTED_EDGE ( 'NONE', *, *, #8586, .T. ) ;
#4572 = DIRECTION ( 'NONE',  ( 0.000000000000000000, 0.000000000000000000, 1.000000000000000000 ) ) ;
#4573 = CIRCLE ( 'NONE', #11070, 0.5590551181102362266 ) ;
#4574 = AXIS2_PLACEMENT_3D ( 'NONE', #70, #2554, #9850 ) ;
#4575 = EDGE_CURVE ( 'NONE', #8847, #13377, #11517, .T. ) ;
#4576 = CARTESIAN_POINT ( 'NONE',  ( -1.943198498587445755, -2.817349890850887384, 0.1717294883501950531 ) ) ;
#4577 = DIRECTION ( 'NONE',  ( 0.000000000000000000, 0.000000000000000000, 1.000000000000000000 ) ) ;
#4578 = CARTESIAN_POINT ( 'NONE',  ( -1.964126537190516331, -2.749515453455444014, -0.1756903148397123138 ) ) ;
#4579 = CARTESIAN_POINT ( 'NONE',  ( -0.2919796512831349111, -0.2952755905511811330, 0.2458576371656082671 ) ) ;
#4580 = CARTESIAN_POINT ( 'NONE',  ( -0.2364476915723336681, -0.1023622047244094474, 0.06377609659094583827 ) ) ;
#4581 = CARTESIAN_POINT ( 'NONE',  ( 6.846450609406462919E-17, 1.409448818897637956, 0.5590551181102362266 ) ) ;
#4582 = CARTESIAN_POINT ( 'NONE',  ( -1.404179464191384508, -0.005170306204214139036, 0.05952236574397579832 ) ) ;
#4583 = DIRECTION ( 'NONE',  ( -1.000000000000000000, 1.734723475976817507E-14, 0.000000000000000000 ) ) ;
#4584 = CARTESIAN_POINT ( 'NONE',  ( 0.4586614173228352742, -0.09448818897637796532, 0.3875520507749248833 ) ) ;
#4585 = CIRCLE ( 'NONE', #6834, 0.03937007874015752140 ) ;
#4586 = ORIENTED_EDGE ( 'NONE', *, *, #15440, .F. ) ;
#4587 = ORIENTED_EDGE ( 'NONE', *, *, #4446, .T. ) ;
#4588 = CIRCLE ( 'NONE', #6557, 0.007874015748031482076 ) ;
#4589 = ORIENTED_EDGE ( 'NONE', *, *, #4351, .T. ) ;
#4590 = EDGE_LOOP ( 'NONE', ( #12988, #7282, #1812, #6801, #11342 ) ) ;
#4591 =( REPRESENTATION_RELATIONSHIP ('NONE','NONE', #8904, #7785 ) REPRESENTATION_RELATIONSHIP_WITH_TRANSFORMATION ( #7226 )SHAPE_REPRESENTATION_RELATIONSHIP( ) );
#4592 = CIRCLE ( 'NONE', #2088, 0.003937007874015724558 ) ;
#4593 = AXIS2_PLACEMENT_3D ( 'NONE', #8619, #3790, #8559 ) ;
#4594 = CARTESIAN_POINT ( 'NONE',  ( -0.03608642540484582190, 0.1707537476062198356, 0.01804586331702636229 ) ) ;
#4595 = VECTOR ( 'NONE', #14298, 39.37007874015748143 ) ;
#4596 = DIRECTION ( 'NONE',  ( 0.000000000000000000, 0.000000000000000000, -1.000000000000000000 ) ) ;
#4597 = CARTESIAN_POINT ( 'NONE',  ( 0.05175539059627461136, 0.06736074103232447818, -0.07475334604056278753 ) ) ;
#4598 = CARTESIAN_POINT ( 'NONE',  ( 0.000000000000000000, 0.000000000000000000, 0.000000000000000000 ) ) ;
#4599 = ORIENTED_EDGE ( 'NONE', *, *, #8540, .T. ) ;
#4600 = CARTESIAN_POINT ( 'NONE',  ( -0.1586168312385622392, -0.003937007874015747977, -0.5890199605878065903 ) ) ;
#4601 = EDGE_CURVE ( 'NONE', #1202, #984, #6558, .T. ) ;
#4602 = DIRECTION ( 'NONE',  ( 0.9966420383350279577, 0.000000000000000000, 0.08188191145424326967 ) ) ;
#4603 = FACE_OUTER_BOUND ( 'NONE', #9452, .T. ) ;
#4604 = ORIENTED_EDGE ( 'NONE', *, *, #9806, .T. ) ;
#4605 = ORIENTED_EDGE ( 'NONE', *, *, #2432, .F. ) ;
#4606 = AXIS2_PLACEMENT_3D ( 'NONE', #3756, #8525, #13300 ) ;
#4607 = AXIS2_PLACEMENT_3D ( 'NONE', #884, #2218, #15061 ) ;
#4608 = CIRCLE ( 'NONE', #870, 0.1535433070866141780 ) ;
#4609 = TOROIDAL_SURFACE ( 'NONE', #4106, 0.5984251968503937480, 0.007874015748031495954 ) ;
#4610 = ORIENTED_EDGE ( 'NONE', *, *, #4801, .T. ) ;
#4611 = AXIS2_PLACEMENT_3D ( 'NONE', #8079, #12867, #12952 ) ;
#4612 = CARTESIAN_POINT ( 'NONE',  ( -0.4749369078591176296, -0.4881889763779528324, 0.3514880584999472424 ) ) ;
#4613 = PRODUCT_DEFINITION_FORMATION_WITH_SPECIFIED_SOURCE ( 'ANY', '', #8027, .NOT_KNOWN. ) ;
#4614 = EDGE_CURVE ( 'NONE', #14592, #851, #3184, .T. ) ;
#4615 = EDGE_CURVE ( 'NONE', #4540, #1832, #3623, .T. ) ;
#4616 = CARTESIAN_POINT ( 'NONE',  ( -0.4330708661417336236, -0.09448818897637796532, 0.4318761856142863120 ) ) ;
#4617 = CARTESIAN_POINT ( 'NONE',  ( -1.947159199436097277, -2.887700558226605541, -0.1349403422227760663 ) ) ;
#4618 = CARTESIAN_POINT ( 'NONE',  ( -0.1181102362204724532, 2.637795275590551825, 0.03937007874015747977 ) ) ;
#4619 = AXIS2_PLACEMENT_3D ( 'NONE', #10751, #6028, #9811 ) ;
#4620 = LINE ( 'NONE', #6013, #3727 ) ;
#4621 = CIRCLE ( 'NONE', #908, 0.003937007874015724558 ) ;
#4622 = CIRCLE ( 'NONE', #7124, 0.03937007874015751446 ) ;
#4623 = CARTESIAN_POINT ( 'NONE',  ( 0.2393297813660762996, -0.4921259842519685179, 0.06089400679746265199 ) ) ;
#4624 = ORIENTED_EDGE ( 'NONE', *, *, #11729, .T. ) ;
#4625 = DIRECTION ( 'NONE',  ( 0.000000000000000000, 0.000000000000000000, 1.000000000000000000 ) ) ;
#4626 = ADVANCED_FACE ( 'NONE', ( #12929 ), #15353, .T. ) ;
#4627 = DIRECTION ( 'NONE',  ( -0.000000000000000000, -1.000000000000000000, -0.000000000000000000 ) ) ;
#4628 = TOROIDAL_SURFACE ( 'NONE', #137, 0.04330708661417328326, 0.003937007874015747977 ) ;
#4629 = CARTESIAN_POINT ( 'NONE',  ( 0.4815353412745612127, 0.000000000000000000, 0.3474236500605469846 ) ) ;
#4630 = CARTESIAN_POINT ( 'NONE',  ( -0.5412478373021294420, 0.000000000000000000, 0.2362233606508100381 ) ) ;
#4631 = VERTEX_POINT ( 'NONE', #10731 ) ;
#4632 = DIRECTION ( 'NONE',  ( 0.000000000000000000, 1.000000000000000000, 0.000000000000000000 ) ) ;
#4633 = ORIENTED_EDGE ( 'NONE', *, *, #8759, .F. ) ;
#4635 = ORIENTED_EDGE ( 'NONE', *, *, #9481, .F. ) ;
#4634 = CIRCLE ( 'NONE', #8391, 0.04330708661417331101 ) ;
#4636 = AXIS2_PLACEMENT_3D ( 'NONE', #10987, #5017, #11048 ) ;
#4637 = ORIENTED_EDGE ( 'NONE', *, *, #12702, .F. ) ;
#4638 = TOROIDAL_SURFACE ( 'NONE', #14656, 0.7007874015748031260, 0.007874015748031495954 ) ;
#4639 = CYLINDRICAL_SURFACE ( 'NONE', #8340, 0.003937007874015721089 ) ;
#4640 = LINE ( 'NONE', #7058, #8395 ) ;
#4641 = AXIS2_PLACEMENT_3D ( 'NONE', #5291, #10091, #13707 ) ;
#4642 = EDGE_CURVE ( 'NONE', #4286, #10078, #14259, .T. ) ;
#4643 = CARTESIAN_POINT ( 'NONE',  ( -1.417802900492933782, -0.04287136159519128881, 0.07874015748031495954 ) ) ;
#4644 = CARTESIAN_POINT ( 'NONE',  ( -0.4342073824196659437, -0.003937007874015747977, 0.4299076816772785525 ) ) ;
#4645 = CONTEXT_DEPENDENT_SHAPE_REPRESENTATION ( #1407, #6766 ) ;
#4646 = DIRECTION ( 'NONE',  ( -0.8660254037844381525, 0.000000000000000000, -0.5000000000000009992 ) ) ;
#4647 = LINE ( 'NONE', #1990, #15390 ) ;
#4648 = ORIENTED_EDGE ( 'NONE', *, *, #6946, .F. ) ;
#4649 = DIRECTION ( 'NONE',  ( 1.000000000000000000, 0.000000000000000000, 0.000000000000000000 ) ) ;
#4650 = EDGE_CURVE ( 'NONE', #9785, #1873, #369, .T. ) ;
#4651 = LINE ( 'NONE', #2292, #15136 ) ;
#4652 = VECTOR ( 'NONE', #13763, 39.37007874015748854 ) ;
#4653 = AXIS2_PLACEMENT_3D ( 'NONE', #3565, #11741, #1003 ) ;
#4654 = CYLINDRICAL_SURFACE ( 'NONE', #12955, 0.1476377952755906220 ) ;
#4655 = VECTOR ( 'NONE', #1185, 39.37007874015748854 ) ;
#4656 = CARTESIAN_POINT ( 'NONE',  ( -1.352291563234457650, 0.1355266887446167634, 0.03937007874015747977 ) ) ;
#4657 = AXIS2_PLACEMENT_3D ( 'NONE', #12037, #7473, #351 ) ;
#4658 = ORIENTED_EDGE ( 'NONE', *, *, #750, .T. ) ;
#4659 = EDGE_CURVE ( 'NONE', #10534, #13283, #7206, .T. ) ;
#4660 = EDGE_LOOP ( 'NONE', ( #4514, #6469, #14892, #14745 ) ) ;
#4661 = ORIENTED_EDGE ( 'NONE', *, *, #2300, .F. ) ;
#4662 = ORIENTED_EDGE ( 'NONE', *, *, #15389, .T. ) ;
#4663 = VECTOR ( 'NONE', #5557, 39.37007874015748143 ) ;
#4664 = CARTESIAN_POINT ( 'NONE',  ( -0.1771653543307086243, -0.02638708502139245488, 0.05905511811023622659 ) ) ;
#4665 = CIRCLE ( 'NONE', #2171, 0.1240157480314959260 ) ;
#4666 = DIRECTION ( 'NONE',  ( 0.000000000000000000, 1.000000000000000000, 0.000000000000000000 ) ) ;
#4667 = CARTESIAN_POINT ( 'NONE',  ( -1.901321527450506199, -2.940045583547485020, -0.05830387289541953677 ) ) ;
#4668 = DIRECTION ( 'NONE',  ( 1.000000000000000000, 0.000000000000000000, 0.000000000000000000 ) ) ;
#4669 = FILL_AREA_STYLE ('',( #15406 ) ) ;
#4670 = CIRCLE ( 'NONE', #6647, 0.003937007874015724558 ) ;
#4671 = PRODUCT_DEFINITION_SHAPE ( 'NONE', 'NONE',  #15488 ) ;
#4672 = FACE_OUTER_BOUND ( 'NONE', #4065, .T. ) ;
#4673 = CARTESIAN_POINT ( 'NONE',  ( -0.1181102362204724254, 2.448818897637795367, 0.03937007874015747977 ) ) ;
#4674 = EDGE_CURVE ( 'NONE', #13441, #11452, #10656, .T. ) ;
#4675 = CARTESIAN_POINT ( 'NONE',  ( -0.09842519685028340570, -0.09842519685039370636, -0.5870514566507987197 ) ) ;
#4676 = DIRECTION ( 'NONE',  ( 1.000000000000000000, 0.000000000000000000, 0.000000000000000000 ) ) ;
#4677 = CYLINDRICAL_SURFACE ( 'NONE', #14171, 0.003937007874015721089 ) ;
#4678 = AXIS2_PLACEMENT_3D ( 'NONE', #1442, #11051, #14359 ) ;
#4679 = EDGE_CURVE ( 'NONE', #12819, #4401, #4608, .T. ) ;
#4680 = ORIENTED_EDGE ( 'NONE', *, *, #5493, .F. ) ;
#4681 = ADVANCED_FACE ( 'NONE', ( #8461 ), #13629, .T. ) ;
#4682 = ORIENTED_EDGE ( 'NONE', *, *, #9953, .F. ) ;
#4683 = EDGE_LOOP ( 'NONE', ( #12719, #14615, #8944 ) ) ;
#4684 = TOROIDAL_SURFACE ( 'NONE', #3675, 0.04330708661417329020, 0.003937007874015747977 ) ;
#4685 = EDGE_LOOP ( 'NONE', ( #4661, #10845, #3985, #15346, #7988, #4831, #10043, #875, #14390, #5370 ) ) ;
#4686 = AXIS2_PLACEMENT_3D ( 'NONE', #3071, #5651, #7851 ) ;
#4687 = DIRECTION ( 'NONE',  ( 1.224646799147353947E-16, 0.000000000000000000, -1.000000000000000000 ) ) ;
#4688 = CIRCLE ( 'NONE', #13440, 0.01968503937007875723 ) ;
#4689 = DIRECTION ( 'NONE',  ( -0.000000000000000000, -1.000000000000000000, -0.000000000000000000 ) ) ;
#4690 = CARTESIAN_POINT ( 'NONE',  ( -0.5445274672588088505, 1.338626482899105241, 0.2461921031270815630 ) ) ;
#4691 = CIRCLE ( 'NONE', #1936, 0.1574803149606299191 ) ;
#4692 = DIRECTION ( 'NONE',  ( -0.000000000000000000, -1.000000000000000000, -0.000000000000000000 ) ) ;
#4693 = ORIENTED_EDGE ( 'NONE', *, *, #8994, .F. ) ;
#4694 = FACE_OUTER_BOUND ( 'NONE', #6641, .T. ) ;
#4695 = DIRECTION ( 'NONE',  ( 0.000000000000000000, 0.000000000000000000, -1.000000000000000000 ) ) ;
#4696 = CIRCLE ( 'NONE', #4441, 0.003937007874015724558 ) ;
#4697 = EDGE_LOOP ( 'NONE', ( #61, #4845, #7127, #2948 ) ) ;
#4698 = ORIENTED_EDGE ( 'NONE', *, *, #15142, .T. ) ;
#4699 = AXIS2_PLACEMENT_3D ( 'NONE', #15097, #9004, #2970 ) ;
#4700 = ORIENTED_EDGE ( 'NONE', *, *, #614, .F. ) ;
#4701 = VECTOR ( 'NONE', #11950, 39.37007874015748143 ) ;
#4702 = CARTESIAN_POINT ( 'NONE',  ( -0.4749369078591176851, -0.4921259842519685179, 0.3514880584999471314 ) ) ;
#4703 = DIRECTION ( 'NONE',  ( 0.000000000000000000, -1.000000000000000000, 0.000000000000000000 ) ) ;
#4704 = CARTESIAN_POINT ( 'NONE',  ( 7.328595018519593763E-17, 0.3070866141732283561, -0.5984251968503937480 ) ) ;
#4705 = CARTESIAN_POINT ( 'NONE',  ( 0.1618514667033794374, -0.4921259842519685179, 0.2161887458866224576 ) ) ;
#4706 = CARTESIAN_POINT ( 'NONE',  ( 0.05114323250695499562, 0.05905511811023622659, -0.08858267716535433989 ) ) ;
#4707 = CARTESIAN_POINT ( 'NONE',  ( -1.919260770607501332, -2.820590578998671827, 0.1479534017216286024 ) ) ;
#4708 = ORIENTED_EDGE ( 'NONE', *, *, #12986, .F. ) ;
#4709 = CARTESIAN_POINT ( 'NONE',  ( -2.003372420862888248, -2.780367306954143469, -0.1578439213240402372 ) ) ;
#4710 = CARTESIAN_POINT ( 'NONE',  ( 0.4625984251968510708, -0.4921259842519685179, 0.3807329531073309070 ) ) ;
#4711 = DIRECTION ( 'NONE',  ( 1.000000000000000000, 0.000000000000000000, 0.000000000000000000 ) ) ;
#4712 = CARTESIAN_POINT ( 'NONE',  ( 0.6864776960422567242, 1.338582677165354395, 0.4645290592786021633 ) ) ;
#4713 = VERTEX_POINT ( 'NONE', #14095 ) ;
#4714 = ADVANCED_FACE ( 'NONE', ( #4772 ), #5342, .T. ) ;
#4715 = ADVANCED_FACE ( 'NONE', ( #3367 ), #13236, .F. ) ;
#4716 = VERTEX_POINT ( 'NONE', #81 ) ;
#4717 = VERTEX_POINT ( 'NONE', #3684 ) ;
#4718 = ORIENTED_EDGE ( 'NONE', *, *, #9455, .F. ) ;
#4719 = VECTOR ( 'NONE', #15279, 39.37007874015748854 ) ;
#4720 = DIRECTION ( 'NONE',  ( 0.4999999999999998335, -0.000000000000000000, 0.8660254037844388186 ) ) ;
#4721 = ADVANCED_FACE ( 'NONE', ( #7040 ), #1099, .T. ) ;
#4722 = CYLINDRICAL_SURFACE ( 'NONE', #12834, 0.5511811023622046335 ) ;
#4723 = CIRCLE ( 'NONE', #6202, 0.1181102362204724532 ) ;
#4724 = CARTESIAN_POINT ( 'NONE',  ( -1.397636319231197355, -0.02569771174688303961, 0.06949204706528756825 ) ) ;
#4725 = CARTESIAN_POINT ( 'NONE',  ( -0.05905511811023624047, 1.043307086614173373, -0.5952259495879738127 ) ) ;
#4726 = DIRECTION ( 'NONE',  ( 0.000000000000000000, 0.000000000000000000, -1.000000000000000000 ) ) ;
#4727 = FACE_OUTER_BOUND ( 'NONE', #12742, .T. ) ;
#4728 = VERTEX_POINT ( 'NONE', #11829 ) ;
#4729 = CARTESIAN_POINT ( 'NONE',  ( 8.148240514011916814E-17, 0.3543307086614172485, 0.6614173228346456046 ) ) ;
#4730 = CARTESIAN_POINT ( 'NONE',  ( 0.6523822077042866763, 1.190944881889763884, 0.4448440199085238467 ) ) ;
#4731 = ADVANCED_FACE ( 'NONE', ( #1024 ), #6082, .F. ) ;
#4732 = DIRECTION ( 'NONE',  ( -0.1209298856814280260, 0.9926610512904576744, 0.000000000000000000 ) ) ;
#4733 = EDGE_CURVE ( 'NONE', #2079, #1202, #2338, .T. ) ;
#4734 = ORIENTED_EDGE ( 'NONE', *, *, #901, .T. ) ;
#4735 = ORIENTED_EDGE ( 'NONE', *, *, #6269, .F. ) ;
#4736 = EDGE_LOOP ( 'NONE', ( #2280, #3519, #13081, #14432 ) ) ;
#4737 = VERTEX_POINT ( 'NONE', #10879 ) ;
#4738 = ADVANCED_FACE ( 'NONE', ( #13388 ), #4054, .T. ) ;
#4739 = VERTEX_POINT ( 'NONE', #11266 ) ;
#4740 = EDGE_CURVE ( 'NONE', #7046, #10377, #9874, .T. ) ;
#4741 = CARTESIAN_POINT ( 'NONE',  ( -1.584115185264708625, 0.1296286773226378586, -0.03937007874015747977 ) ) ;
#4742 = CARTESIAN_POINT ( 'NONE',  ( -1.234181327013985197, 0.1355266887446167634, 0.03937007874015747977 ) ) ;
#4743 = CARTESIAN_POINT ( 'NONE',  ( -0.3117681530218310848, -0.2952755905511811330, 0.2981971199768678193 ) ) ;
#4744 = SURFACE_STYLE_FILL_AREA ( #4669 ) ;
#4745 = DIRECTION ( 'NONE',  ( 0.000000000000000000, 0.000000000000000000, 1.000000000000000000 ) ) ;
#4746 = DIRECTION ( 'NONE',  ( -0.000000000000000000, -0.000000000000000000, -1.000000000000000000 ) ) ;
#4747 = CYLINDRICAL_SURFACE ( 'NONE', #9125, 0.03937007874015747977 ) ;
#4748 = CARTESIAN_POINT ( 'NONE',  ( -0.2362204724409448231, -0.02638708502139245488, 0.03937007874015747977 ) ) ;
#4749 = CARTESIAN_POINT ( 'NONE',  ( 8.630384923125046426E-17, 0.3149606299212598381, -0.7007874015748031260 ) ) ;
#4750 = ORIENTED_EDGE ( 'NONE', *, *, #11500, .T. ) ;
#4751 = ORIENTED_EDGE ( 'NONE', *, *, #6055, .T. ) ;
#4752 = ORIENTED_EDGE ( 'NONE', *, *, #10931, .T. ) ;
#4753 = VERTEX_POINT ( 'NONE', #1721 ) ;
#4754 = EDGE_CURVE ( 'NONE', #5666, #5246, #11554, .T. ) ;
#4755 = ADVANCED_FACE ( 'NONE', ( #13534, #12291 ), #7430, .F. ) ;
#4756 = CARTESIAN_POINT ( 'NONE',  ( -1.181102362204724310, -0.1240157480314959815, -0.02559055118110236185 ) ) ;
#4757 = CARTESIAN_POINT ( 'NONE',  ( -0.05639125304298656799, 0.1674615591801701664, 0.03403793048618138084 ) ) ;
#4758 = EDGE_CURVE ( 'NONE', #2746, #4753, #13868, .T. ) ;
#4759 = CARTESIAN_POINT ( 'NONE',  ( -1.437672431148612429, -0.06355280397547365123, 0.1968503937007874127 ) ) ;
#4760 = PLANE ( 'NONE',  #11839 ) ;
#4761 = CARTESIAN_POINT ( 'NONE',  ( -0.05114323250695500950, 0.05905511811023622659, 0.08858267716535433989 ) ) ;
#4762 = VERTEX_POINT ( 'NONE', #539 ) ;
#4763 = FACE_OUTER_BOUND ( 'NONE', #760, .T. ) ;
#4764 = CARTESIAN_POINT ( 'NONE',  ( 0.1023622047244638067, -0.4921259842519685179, -0.2472069366676780122 ) ) ;
#4765 = CARTESIAN_POINT ( 'NONE',  ( -0.2393297813659119588, -0.4881889763779528324, 0.06089400679736758221 ) ) ;
#4766 = ORIENTED_EDGE ( 'NONE', *, *, #11607, .T. ) ;
#4767 = ORIENTED_EDGE ( 'NONE', *, *, #4515, .T. ) ;
#4768 = ORIENTED_EDGE ( 'NONE', *, *, #9328, .T. ) ;
#4769 = LINE ( 'NONE', #2266, #6117 ) ;
#4770 = CARTESIAN_POINT ( 'NONE',  ( -1.580080891953811628, 0.1020406297922291511, 0.07874015748031495954 ) ) ;
#4771 = CARTESIAN_POINT ( 'NONE',  ( -1.927122758893819121, -2.943756582367311747, -0.04519362198192262287 ) ) ;
#4772 = FACE_OUTER_BOUND ( 'NONE', #3133, .T. ) ;
#4773 = ADVANCED_FACE ( 'NONE', ( #12146 ), #1413, .F. ) ;
#4774 = CARTESIAN_POINT ( 'NONE',  ( 0.000000000000000000, 0.06496062992125986590, -0.03937007874015747977 ) ) ;
#4775 = CARTESIAN_POINT ( 'NONE',  ( -0.06692913385815749128, -0.4881889763779528324, -0.2377126739438355507 ) ) ;
#4776 = DIRECTION ( 'NONE',  ( -0.4999999999999998335, -0.000000000000000000, -0.8660254037844388186 ) ) ;
#4777 = ORIENTED_EDGE ( 'NONE', *, *, #13134, .F. ) ;
#4778 = CARTESIAN_POINT ( 'NONE',  ( -1.991673489327364432, -2.812934328829368003, 0.1541855436941547697 ) ) ;
#4779 = CARTESIAN_POINT ( 'NONE',  ( 0.5379290338433416752, -0.09842519685039370636, 0.2423824958184916112 ) ) ;
#4780 = CARTESIAN_POINT ( 'NONE',  ( 0.5412723129863803440, 1.340161119985692428, 0.2430722610364096370 ) ) ;
#4781 = ORIENTED_EDGE ( 'NONE', *, *, #424, .T. ) ;
#4782 = EDGE_LOOP ( 'NONE', ( #1855, #7764, #11399, #9027, #5505, #3787, #12199 ) ) ;
#4783 = CARTESIAN_POINT ( 'NONE',  ( 0.1763376553817700698, -0.09842519685039370636, 0.1699995694788709322 ) ) ;
#4784 = CARTESIAN_POINT ( 'NONE',  ( -1.399712684983831723, -0.02644324255144274438, 0.07681107545239827805 ) ) ;
#4785 = DIRECTION ( 'NONE',  ( 0.1209298856814283590, -0.9926610512904576744, 0.000000000000000000 ) ) ;
#4786 = LINE ( 'NONE', #10811, #11193 ) ;
#4787 = EDGE_CURVE ( 'NONE', #713, #6899, #1489, .T. ) ;
#4788 = CARTESIAN_POINT ( 'NONE',  ( 0.000000000000000000, 8.003460918938271148E-19, 0.04330708661417326938 ) ) ;
#4789 = ORIENTED_EDGE ( 'NONE', *, *, #9273, .F. ) ;
#4790 = CARTESIAN_POINT ( 'NONE',  ( -0.1552072824047652788, -0.003937007874015747977, -0.5870514566507987197 ) ) ;
#4791 = CARTESIAN_POINT ( 'NONE',  ( -0.3441669734936866343, 2.010494531933507467, 0.03937007874015747977 ) ) ;
#4792 = CARTESIAN_POINT ( 'NONE',  ( -0.05074681685833758865, -0.1845569960845552526, 0.03403827111684314816 ) ) ;
#4793 = EDGE_CURVE ( 'NONE', #7774, #2681, #6398, .T. ) ;
#4794 = VERTEX_POINT ( 'NONE', #6169 ) ;
#4795 = EDGE_LOOP ( 'NONE', ( #6233, #6996, #8326, #578 ) ) ;
#4796 = ORIENTED_EDGE ( 'NONE', *, *, #3703, .F. ) ;
#4797 = ORIENTED_EDGE ( 'NONE', *, *, #5024, .T. ) ;
#4798 = CARTESIAN_POINT ( 'NONE',  ( -0.1734555655881918346, -0.4881889763779528324, 0.1728816592724491952 ) ) ;
#4799 = DIRECTION ( 'NONE',  ( 0.000000000000000000, 0.000000000000000000, 1.000000000000000000 ) ) ;
#4800 = CARTESIAN_POINT ( 'NONE',  ( -1.898742709278110841, -2.947125287889049261, -0.02947887163950623987 ) ) ;
#4801 = EDGE_CURVE ( 'NONE', #4326, #3768, #478, .T. ) ;
#4802 = DIRECTION ( 'NONE',  ( 1.110223024625156540E-16, 0.8219459448134283086, -0.5695655044020488944 ) ) ;
#4803 = DIRECTION ( 'NONE',  ( 0.8221763679505059708, -0.000000000000000000, 0.5692328345973325376 ) ) ;
#4804 = ADVANCED_FACE ( 'NONE', ( #5059 ), #7349, .F. ) ;
#4805 = DIRECTION ( 'NONE',  ( -0.000000000000000000, -1.000000000000000000, -0.000000000000000000 ) ) ;
#4806 = LINE ( 'NONE', #13348, #14668 ) ;
#4807 = CARTESIAN_POINT ( 'NONE',  ( 6.846450609406462919E-17, 1.622047244094488638, -0.5590551181102362266 ) ) ;
#4808 = DIRECTION ( 'NONE',  ( -0.000000000000000000, -1.000000000000000000, -0.000000000000000000 ) ) ;
#4809 = ADVANCED_FACE ( 'NONE', ( #10018 ), #8365, .T. ) ;
#4810 = DIRECTION ( 'NONE',  ( 0.000000000000000000, 0.5840537863397233798, -0.8117149589986825120 ) ) ;
#4811 = CARTESIAN_POINT ( 'NONE',  ( -1.181102362204724310, -0.1240157480314959815, 0.02559055118110236185 ) ) ;
#4812 = VERTEX_POINT ( 'NONE', #9866 ) ;
#4813 = ORIENTED_EDGE ( 'NONE', *, *, #9610, .T. ) ;
#4814 = EDGE_LOOP ( 'NONE', ( #533, #5643, #4190, #1664, #1448, #2691, #5597, #3408 ) ) ;
#4815 = ORIENTED_EDGE ( 'NONE', *, *, #2835, .T. ) ;
#4816 = EDGE_CURVE ( 'NONE', #6744, #5934, #2844, .T. ) ;
#4817 = CARTESIAN_POINT ( 'NONE',  ( 0.000000000000000000, 2.433070866141732846, 0.000000000000000000 ) ) ;
#4818 = CARTESIAN_POINT ( 'NONE',  ( -0.05905511811012598145, -0.1023622047244094474, -0.2377126739438355507 ) ) ;
#4819 = EDGE_CURVE ( 'NONE', #13305, #3451, #7111, .T. ) ;
#4820 = CARTESIAN_POINT ( 'NONE',  ( -1.181102362204724310, -0.1279527559055117225, 0.02952755905511811330 ) ) ;
#4821 = CARTESIAN_POINT ( 'NONE',  ( -0.2393297813659119588, -0.4921259842519685179, 0.06089400679736759608 ) ) ;
#4822 = CARTESIAN_POINT ( 'NONE',  ( 0.000000000000000000, 0.3070866141732283561, -0.5905511811023621549 ) ) ;
#4823 = AXIS2_PLACEMENT_3D ( 'NONE', #13089, #11939, #2356 ) ;
#4824 = AXIS2_PLACEMENT_3D ( 'NONE', #4201, #10301, #11171 ) ;
#4825 = CARTESIAN_POINT ( 'NONE',  ( 0.000000000000000000, 1.622047244094488638, 0.000000000000000000 ) ) ;
#4826 = EDGE_LOOP ( 'NONE', ( #14973, #8035, #4766, #4880 ) ) ;
#4827 = CARTESIAN_POINT ( 'NONE',  ( 0.4586614173228352742, -0.1023622047244094474, 0.3875520507749248833 ) ) ;
#4828 = ADVANCED_FACE ( 'NONE', ( #13613 ), #6480, .F. ) ;
#4829 = CARTESIAN_POINT ( 'NONE',  ( -2.182693454834259139, -1.630005269948474389, -0.08366141732283423338 ) ) ;
#4830 = CARTESIAN_POINT ( 'NONE',  ( 0.05905511811029059283, -0.1023622047244094474, -0.2377126739437405434 ) ) ;
#4831 = ORIENTED_EDGE ( 'NONE', *, *, #8258, .T. ) ;
#4832 = ORIENTED_EDGE ( 'NONE', *, *, #6413, .T. ) ;
#4833 = EDGE_CURVE ( 'NONE', #10116, #13891, #2564, .T. ) ;
#4834 = ORIENTED_EDGE ( 'NONE', *, *, #12581, .F. ) ;
#4835 = AXIS2_PLACEMENT_3D ( 'NONE', #8351, #7184, #7407 ) ;
#4836 = CIRCLE ( 'NONE', #6317, 0.04330708661417329020 ) ;
#4837 = DIRECTION ( 'NONE',  ( 0.000000000000000000, 0.000000000000000000, 1.000000000000000000 ) ) ;
#4838 = CIRCLE ( 'NONE', #13591, 0.01968503937007875723 ) ;
#4839 = TOROIDAL_SURFACE ( 'NONE', #12350, 0.04330708661417326938, 0.003937007874015747977 ) ;
#4840 = CARTESIAN_POINT ( 'NONE',  ( 0.09842519685044814892, -0.2952755905511811330, -0.4190977005962941426 ) ) ;
#4841 = DIRECTION ( 'NONE',  ( -0.000000000000000000, -1.000000000000000000, -0.000000000000000000 ) ) ;
#4842 = CARTESIAN_POINT ( 'NONE',  ( -2.156938452685383645, -2.012428322114202306, 0.1097289591314137142 ) ) ;
#4843 = DIRECTION ( 'NONE',  ( -1.000000000000000000, 0.000000000000000000, 0.000000000000000000 ) ) ;
#4844 = CARTESIAN_POINT ( 'NONE',  ( -1.926823381055724260, -2.799657869570562063, 0.1538728403396771027 ) ) ;
#4845 = ORIENTED_EDGE ( 'NONE', *, *, #9761, .T. ) ;
#4846 = DIRECTION ( 'NONE',  ( -0.9482728725910103407, -0.3174563893009453297, 0.000000000000000000 ) ) ;
#4847 = CARTESIAN_POINT ( 'NONE',  ( -2.080881322745466999, -1.632190302820504479, 0.08366141732283424726 ) ) ;
#4848 = EDGE_CURVE ( 'NONE', #3695, #8997, #366, .T. ) ;
#4849 = AXIS2_PLACEMENT_3D ( 'NONE', #282, #934, #13210 ) ;
#4850 = CIRCLE ( 'NONE', #12112, 0.003937007874015724558 ) ;
#4851 = CARTESIAN_POINT ( 'NONE',  ( -0.06155496847469428545, 0.1461038053415527060, -0.05764730824460249231 ) ) ;
#4852 = AXIS2_PLACEMENT_3D ( 'NONE', #12967, #6926, #985 ) ;
#4853 = ORIENTED_EDGE ( 'NONE', *, *, #10764, .T. ) ;
#4854 = VERTEX_POINT ( 'NONE', #10405 ) ;
#4855 = VECTOR ( 'NONE', #773, 39.37007874015748143 ) ;
#4856 = DIRECTION ( 'NONE',  ( 1.000000000000000000, 0.000000000000000000, 0.000000000000000000 ) ) ;
#4857 = EDGE_CURVE ( 'NONE', #11091, #14143, #11108, .T. ) ;
#4858 = ORIENTED_EDGE ( 'NONE', *, *, #998, .F. ) ;
#4859 = ORIENTED_EDGE ( 'NONE', *, *, #550, .T. ) ;
#4860 = DIRECTION ( 'NONE',  ( -0.000000000000000000, 1.000000000000000000, -0.000000000000000000 ) ) ;
#4861 = AXIS2_PLACEMENT_3D ( 'NONE', #11151, #13501, #9039 ) ;
#4862 = AXIS2_PLACEMENT_3D ( 'NONE', #6477, #8691, #11264 ) ;
#4863 = CIRCLE ( 'NONE', #6862, 0.03937007874015752140 ) ;
#4864 = CARTESIAN_POINT ( 'NONE',  ( -1.406518536868439195, -0.03328691616031433792, 0.04686241403499121633 ) ) ;
#4865 = DIRECTION ( 'NONE',  ( -0.000000000000000000, -1.000000000000000000, -0.000000000000000000 ) ) ;
#4866 = CONTEXT_DEPENDENT_SHAPE_REPRESENTATION ( #4897, #9166 ) ;
#4867 = CARTESIAN_POINT ( 'NONE',  ( 5.303588500244447761E-18, 0.003937007874015749712, -0.04330708661417326938 ) ) ;
#4868 = CARTESIAN_POINT ( 'NONE',  ( 0.2393297813660762718, -0.1023622047244094474, 0.06089400679746260342 ) ) ;
#4869 = AXIS2_PLACEMENT_3D ( 'NONE', #13866, #491, #4070 ) ;
#4870 = CARTESIAN_POINT ( 'NONE',  ( -0.1734555655881918346, -0.4921259842519685179, 0.1728816592724491952 ) ) ;
#4871 = VERTEX_POINT ( 'NONE', #4364 ) ;
#4872 = DIRECTION ( 'NONE',  ( -0.8144815189573203495, 0.5801894994542524664, -1.283760644411384396E-16 ) ) ;
#4873 = CARTESIAN_POINT ( 'NONE',  ( 0.05114323250695503031, 0.000000000000000000, 0.08858267716535433989 ) ) ;
#4874 = CARTESIAN_POINT ( 'NONE',  ( -0.06762554849860653861, -0.1867557816141674765, 0.05879187219561141792 ) ) ;
#4875 = LINE ( 'NONE', #1512, #8675 ) ;
#4876 = CIRCLE ( 'NONE', #13895, 0.003937007874015721089 ) ;
#4877 = CIRCLE ( 'NONE', #10884, 0.003937007874015741038 ) ;
#4878 = AXIS2_PLACEMENT_3D ( 'NONE', #9453, #7164, #12592 ) ;
#4879 = ORIENTED_EDGE ( 'NONE', *, *, #2157, .T. ) ;
#4880 = ORIENTED_EDGE ( 'NONE', *, *, #6451, .T. ) ;
#4881 = EDGE_LOOP ( 'NONE', ( #7931, #14271, #5145 ) ) ;
#4882 = CIRCLE ( 'NONE', #9653, 0.03543307086614173179 ) ;
#4883 = VERTEX_POINT ( 'NONE', #12599 ) ;
#4884 = FACE_OUTER_BOUND ( 'NONE', #9, .T. ) ;
#4885 = CARTESIAN_POINT ( 'NONE',  ( 0.4330708661417309036, 0.000000000000000000, 0.4279391777402732910 ) ) ;
#4886 = CARTESIAN_POINT ( 'NONE',  ( 0.000000000000000000, 0.000000000000000000, -0.5905511811023621549 ) ) ;
#4887 = DIRECTION ( 'NONE',  ( 2.053912595556538811E-15, -0.1506948608623633334, 0.9885803249658942082 ) ) ;
#4888 = TOROIDAL_SURFACE ( 'NONE', #7153, 0.7007874015748031260, 0.007874015748031495954 ) ;
#4889 = CARTESIAN_POINT ( 'NONE',  ( -0.6582248459352179060, -0.2952755905511811330, -0.3018834747714004840 ) ) ;
#4890 = CIRCLE ( 'NONE', #4382, 0.003937007874015724558 ) ;
#4891 = CARTESIAN_POINT ( 'NONE',  ( -0.03802712947489397116, 0.1704066588063142818, 0.02158149019474815342 ) ) ;
#4892 = AXIS2_PLACEMENT_3D ( 'NONE', #4483, #8248, #15459 ) ;
#4893 = CARTESIAN_POINT ( 'NONE',  ( 0.000000000000000000, 0.000000000000000000, 0.000000000000000000 ) ) ;
#4894 = CARTESIAN_POINT ( 'NONE',  ( 7.328595018519593763E-17, 1.653543307086614567, 0.5984251968503937480 ) ) ;
#4895 = DIRECTION ( 'NONE',  ( -0.9967194639908912857, 0.08093398607328357308, 0.000000000000000000 ) ) ;
#4896 = CIRCLE ( 'NONE', #9413, 0.003937007874015724558 ) ;
#4897 =( REPRESENTATION_RELATIONSHIP ('NONE','NONE', #8904, #11075 ) REPRESENTATION_RELATIONSHIP_WITH_TRANSFORMATION ( #6026 )SHAPE_REPRESENTATION_RELATIONSHIP( ) );
#4898 = FACE_OUTER_BOUND ( 'NONE', #10170, .T. ) ;
#4899 = DIRECTION ( 'NONE',  ( 0.5000000000000041078, 0.000000000000000000, 0.8660254037844362651 ) ) ;
#4900 = ORIENTED_EDGE ( 'NONE', *, *, #11557, .T. ) ;
#4901 = VECTOR ( 'NONE', #799, 39.37007874015748143 ) ;
#4902 = VERTEX_POINT ( 'NONE', #1867 ) ;
#4903 = CIRCLE ( 'NONE', #4653, 0.003937007874015758385 ) ;
#4904 = EDGE_CURVE ( 'NONE', #9513, #238, #3041, .T. ) ;
#4905 = AXIS2_PLACEMENT_3D ( 'NONE', #11397, #449, #3965 ) ;
#4906 = ORIENTED_EDGE ( 'NONE', *, *, #7223, .F. ) ;
#4907 = TOROIDAL_SURFACE ( 'NONE', #10169, 0.04330708661417328326, 0.003937007874015747977 ) ;
#4908 = EDGE_CURVE ( 'NONE', #14540, #10513, #1789, .T. ) ;
#4909 = DIRECTION ( 'NONE',  ( 1.770352960217306852E-32, 1.000000000000000000, -1.224646799147353207E-16 ) ) ;
#4910 = LINE ( 'NONE', #8510, #13985 ) ;
#4911 = CARTESIAN_POINT ( 'NONE',  ( 0.4572203724260462399, -0.1023622047244094474, 0.3821739980041199969 ) ) ;
#4912 = CARTESIAN_POINT ( 'NONE',  ( 0.4788739157331329821, -0.1023622047244094474, 0.3446689608323529885 ) ) ;
#4913 = DIRECTION ( 'NONE',  ( 0.8660254037844383745, 0.000000000000000000, -0.5000000000000004441 ) ) ;
#4914 = AXIS2_PLACEMENT_3D ( 'NONE', #2477, #354, #11067 ) ;
#4915 = CARTESIAN_POINT ( 'NONE',  ( 6.750021727583836750E-17, 0.04724409448818898960, 0.5511811023622046335 ) ) ;
#4916 = DIRECTION ( 'NONE',  ( -0.000000000000000000, -1.000000000000000000, -0.000000000000000000 ) ) ;
#4917 = CARTESIAN_POINT ( 'NONE',  ( -0.09842519685028335019, -0.2952755905511811330, -0.4190977005962941981 ) ) ;
#4918 = DIRECTION ( 'NONE',  ( 8.673617379884028076E-17, -1.000000000000000000, 0.000000000000000000 ) ) ;
#4919 = AXIS2_PLACEMENT_3D ( 'NONE', #647, #12313, #14817 ) ;
#4920 = ORIENTED_EDGE ( 'NONE', *, *, #6921, .T. ) ;
#4921 = ORIENTED_EDGE ( 'NONE', *, *, #12573, .F. ) ;
#4922 = AXIS2_PLACEMENT_3D ( 'NONE', #7772, #10136, #13664 ) ;
#4923 = EDGE_CURVE ( 'NONE', #14663, #10930, #3620, .T. ) ;
#4924 = ORIENTED_EDGE ( 'NONE', *, *, #2126, .F. ) ;
#4925 = PRESENTATION_LAYER_ASSIGNMENT (  '', '', ( #2928 ) ) ;
#4926 = CARTESIAN_POINT ( 'NONE',  ( -1.580259682937477539, 0.1018956540319142512, 0.04477369844320258641 ) ) ;
#4927 = ADVANCED_FACE ( 'NONE', ( #15098 ), #3270, .F. ) ;
#4928 = EDGE_CURVE ( 'NONE', #12623, #10078, #15117, .T. ) ;
#4929 = AXIS2_PLACEMENT_3D ( 'NONE', #7745, #13712, #12535 ) ;
#4930 = DIRECTION ( 'NONE',  ( 0.000000000000000000, 0.000000000000000000, 1.000000000000000000 ) ) ;
#4931 = LINE ( 'NONE', #311, #15127 ) ;
#4932 = VECTOR ( 'NONE', #8234, 39.37007874015748143 ) ;
#4933 = DIRECTION ( 'NONE',  ( 0.000000000000000000, 1.000000000000000000, -0.000000000000000000 ) ) ;
#4934 = CARTESIAN_POINT ( 'NONE',  ( 0.000000000000000000, 0.03149606299212599769, 0.000000000000000000 ) ) ;
#4935 = CARTESIAN_POINT ( 'NONE',  ( -1.180847381077431146, 0.3433074774436084553, -0.04453711288976486965 ) ) ;
#4936 = ORIENTED_EDGE ( 'NONE', *, *, #11508, .T. ) ;
#4937 = CARTESIAN_POINT ( 'NONE',  ( -0.09842519685028361387, -0.4921259842519685179, -3.421829314686310476E-17 ) ) ;
#4938 = DIRECTION ( 'NONE',  ( -0.000000000000000000, -1.000000000000000000, 4.956352788505160310E-16 ) ) ;
#4939 = CARTESIAN_POINT ( 'NONE',  ( 0.5403775459648877399, 1.343094183513034778, 0.2394881783597540836 ) ) ;
#4940 = ORIENTED_EDGE ( 'NONE', *, *, #7525, .F. ) ;
#4941 = EDGE_LOOP ( 'NONE', ( #9242, #1530, #13526, #9681 ) ) ;
#4942 = AXIS2_PLACEMENT_3D ( 'NONE', #1441, #5018, #12253 ) ;
#4943 = ORIENTED_EDGE ( 'NONE', *, *, #4307, .T. ) ;
#4944 = DIRECTION ( 'NONE',  ( -0.8660254037844405950, -7.511572993685826514E-15, -0.4999999999999967248 ) ) ;
#4945 = EDGE_CURVE ( 'NONE', #1542, #14687, #4085, .T. ) ;
#4946 = AXIS2_PLACEMENT_3D ( 'NONE', #7789, #4266, #12341 ) ;
#4947 = CARTESIAN_POINT ( 'NONE',  ( 8.678599364036360127E-17, 0.5826771653543306728, 0.7086614173228346081 ) ) ;
#4948 = DIRECTION ( 'NONE',  ( 0.000000000000000000, 0.000000000000000000, -1.000000000000000000 ) ) ;
#4949 = AXIS2_PLACEMENT_3D ( 'NONE', #319, #20, #9876 ) ;
#4950 = DIRECTION ( 'NONE',  ( -0.000000000000000000, 1.000000000000000000, -0.000000000000000000 ) ) ;
#4951 = CARTESIAN_POINT ( 'NONE',  ( -0.05809364415030902895, 0.1671978997630559072, -0.03476146466084938796 ) ) ;
#4952 = ORIENTED_EDGE ( 'NONE', *, *, #12225, .F. ) ;
#4953 = CARTESIAN_POINT ( 'NONE',  ( -0.1574803149606299191, -0.09448818897637796532, -0.5870514566507987197 ) ) ;
#4954 = EDGE_CURVE ( 'NONE', #3736, #2187, #112, .T. ) ;
#4955 = CARTESIAN_POINT ( 'NONE',  ( 0.05905511811029064834, -0.1023622047244094474, -0.5909884645248143498 ) ) ;
#4956 = CARTESIAN_POINT ( 'NONE',  ( -0.03726694595799353443, -0.1642704670929807653, 0.04781780748315901663 ) ) ;
#4957 = AXIS2_PLACEMENT_3D ( 'NONE', #5629, #10427, #12773 ) ;
#4958 = ORIENTED_EDGE ( 'NONE', *, *, #165, .F. ) ;
#4959 = ORIENTED_EDGE ( 'NONE', *, *, #10498, .F. ) ;
#4960 = ORIENTED_EDGE ( 'NONE', *, *, #1427, .T. ) ;
#4961 = ADVANCED_FACE ( 'NONE', ( #6782 ), #12529, .T. ) ;
#4962 = SPHERICAL_SURFACE ( 'NONE', #6386, 0.01968503937007873988 ) ;
#4963 = DIRECTION ( 'NONE',  ( -0.000000000000000000, -1.000000000000000000, 0.000000000000000000 ) ) ;
#4964 = DIRECTION ( 'NONE',  ( 0.4999999999999966693, 0.000000000000000000, 0.8660254037844405950 ) ) ;
#4965 = DIRECTION ( 'NONE',  ( 0.7497915094135898517, 0.5004167495348750272, -0.4328923297960365901 ) ) ;
#4966 =( NAMED_UNIT ( * ) SI_UNIT ( $, .STERADIAN. ) SOLID_ANGLE_UNIT ( ) );
#4967 = LINE ( 'NONE', #6046, #14868 ) ;
#4968 = CARTESIAN_POINT ( 'NONE',  ( -0.1023622047242991467, -0.4921259842519685179, -0.5870514566507987197 ) ) ;
#4969 = CARTESIAN_POINT ( 'NONE',  ( -1.957251767100264495, -2.772329397581817734, -0.1771653543307079026 ) ) ;
#4970 = CARTESIAN_POINT ( 'NONE',  ( 0.000000000000000000, -0.4921259842519685179, 0.000000000000000000 ) ) ;
#4971 = CARTESIAN_POINT ( 'NONE',  ( 1.137795275590550936, 4.097147066950659020E-16, 0.02559055118110236185 ) ) ;
#4972 = ORIENTED_EDGE ( 'NONE', *, *, #13510, .F. ) ;
#4973 = ORIENTED_EDGE ( 'NONE', *, *, #7023, .F. ) ;
#4974 = VERTEX_POINT ( 'NONE', #15187 ) ;
#4975 = DIRECTION ( 'NONE',  ( -0.000000000000000000, 1.000000000000000000, 0.000000000000000000 ) ) ;
#4976 = CARTESIAN_POINT ( 'NONE',  ( -0.06692913385815735250, -0.1023622047244094474, -0.5870514566507987197 ) ) ;
#4977 = DIRECTION ( 'NONE',  ( 0.000000000000000000, -1.734723475976802677E-14, -1.000000000000000000 ) ) ;
#4978 = EDGE_CURVE ( 'NONE', #8620, #12332, #13250, .T. ) ;
#4979 = CARTESIAN_POINT ( 'NONE',  ( -1.181102362204724310, 0.1240157480314959815, 0.02559055118110236185 ) ) ;
#4980 = CARTESIAN_POINT ( 'NONE',  ( 1.181102362204724310, 4.044111181948214319E-16, -0.02559055118110236185 ) ) ;
#4981 = DIRECTION ( 'NONE',  ( -0.000000000000000000, 0.000000000000000000, 1.000000000000000000 ) ) ;
#4982 = EDGE_CURVE ( 'NONE', #2526, #9714, #1613, .T. ) ;
#4983 = FACE_OUTER_BOUND ( 'NONE', #15229, .T. ) ;
#4984 = CARTESIAN_POINT ( 'NONE',  ( 0.4861941749621881415, 1.043307086614173373, 0.3488953144687809704 ) ) ;
#4985 = ORIENTED_EDGE ( 'NONE', *, *, #2244, .F. ) ;
#4986 = EDGE_CURVE ( 'NONE', #12009, #13441, #10369, .T. ) ;
#4987 = ORIENTED_EDGE ( 'NONE', *, *, #14159, .T. ) ;
#4988 = ORIENTED_EDGE ( 'NONE', *, *, #1305, .T. ) ;
#4989 = ORIENTED_EDGE ( 'NONE', *, *, #5076, .T. ) ;
#4990 = ORIENTED_EDGE ( 'NONE', *, *, #165, .T. ) ;
#4991 = CARTESIAN_POINT ( 'NONE',  ( 7.328595018519593763E-17, 0.3149606299212598381, -0.5984251968503937480 ) ) ;
#4992 = CARTESIAN_POINT ( 'NONE',  ( 0.000000000000000000, -0.09842519685039370636, -0.1614173228346456879 ) ) ;
#4993 = CARTESIAN_POINT ( 'NONE',  ( 0.5894146648244296127, -0.09842519685039370636, 0.1571437749735215827 ) ) ;
#4994 = CARTESIAN_POINT ( 'NONE',  ( 8.100026073100603114E-17, 1.425196850393700920, 0.6614173228346456046 ) ) ;
#4995 = ADVANCED_FACE ( 'NONE', ( #8041 ), #7589, .T. ) ;
#4996 = DIRECTION ( 'NONE',  ( 0.8660254037844389297, 0.000000000000000000, -0.4999999999999996669 ) ) ;
#4997 = CARTESIAN_POINT ( 'NONE',  ( 0.000000000000000000, 0.000000000000000000, 0.05905511811023622659 ) ) ;
#4998 = CARTESIAN_POINT ( 'NONE',  ( -1.882391615595319756, -2.915690172171810257, 0.04572057578730489430 ) ) ;
#4999 = EDGE_CURVE ( 'NONE', #7929, #11495, #5845, .T. ) ;
#5000 = EDGE_LOOP ( 'NONE', ( #3904, #1978, #6203, #3275 ) ) ;
#5001 = CARTESIAN_POINT ( 'NONE',  ( -1.950427925093563220, -2.919740984733180333, -0.07234829986380927891 ) ) ;
#5002 = DIRECTION ( 'NONE',  ( 0.5000000000000004441, 0.000000000000000000, -0.8660254037844384856 ) ) ;
#5003 = ORIENTED_EDGE ( 'NONE', *, *, #11748, .T. ) ;
#5004 = EDGE_CURVE ( 'NONE', #8246, #3213, #9371, .T. ) ;
#5005 = EDGE_LOOP ( 'NONE', ( #4292, #12268, #6015, #10184, #14292, #6120, #9669, #1038, #406, #6880 ) ) ;
#5006 = EDGE_LOOP ( 'NONE', ( #8806, #8260, #14475, #4552 ) ) ;
#5007 = DIRECTION ( 'NONE',  ( 0.000000000000000000, 0.000000000000000000, 1.000000000000000000 ) ) ;
#5008 = CARTESIAN_POINT ( 'NONE',  ( 0.000000000000000000, 0.5433070866141731514, 0.000000000000000000 ) ) ;
#5009 = DIRECTION ( 'NONE',  ( 0.000000000000000000, 1.000000000000000000, -0.000000000000000000 ) ) ;
#5010 = DIRECTION ( 'NONE',  ( 0.8011800915434521553, -0.5984233124757303290, 0.000000000000000000 ) ) ;
#5011 = FACE_OUTER_BOUND ( 'NONE', #10273, .T. ) ;
#5012 = CARTESIAN_POINT ( 'NONE',  ( 0.7455328141524921737, 1.190944881889763884, 0.3622425942646917418 ) ) ;
#5013 = EDGE_CURVE ( 'NONE', #4456, #2187, #9615, .T. ) ;
#5014 = ORIENTED_EDGE ( 'NONE', *, *, #5861, .T. ) ;
#5015 = DIRECTION ( 'NONE',  ( -0.000000000000000000, -1.000000000000000000, -0.000000000000000000 ) ) ;
#5016 = DIRECTION ( 'NONE',  ( -3.469446951953635015E-14, 0.000000000000000000, -1.000000000000000000 ) ) ;
#5017 = DIRECTION ( 'NONE',  ( 0.000000000000000000, 0.000000000000000000, 1.000000000000000000 ) ) ;
#5018 = DIRECTION ( 'NONE',  ( -0.4999999999999986122, -0.000000000000000000, -0.8660254037844394848 ) ) ;
#5019 = EDGE_CURVE ( 'NONE', #13544, #7994, #4967, .T. ) ;
#5020 = ORIENTED_EDGE ( 'NONE', *, *, #10108, .F. ) ;
#5021 = ORIENTED_EDGE ( 'NONE', *, *, #944, .T. ) ;
#5022 = ORIENTED_EDGE ( 'NONE', *, *, #13524, .T. ) ;
#5023 = ORIENTED_EDGE ( 'NONE', *, *, #4424, .F. ) ;
#5024 = EDGE_CURVE ( 'NONE', #3640, #9446, #13363, .T. ) ;
#5025 = DIRECTION ( 'NONE',  ( -0.000000000000000000, -1.000000000000000000, -0.000000000000000000 ) ) ;
#5026 = FACE_OUTER_BOUND ( 'NONE', #6966, .T. ) ;
#5027 = CARTESIAN_POINT ( 'NONE',  ( 0.000000000000000000, 0.5511811023622046335, 0.000000000000000000 ) ) ;
#5028 = DIRECTION ( 'NONE',  ( 0.7279172371620082904, 0.5417705490241228050, -0.4202632128232604569 ) ) ;
#5029 = PRODUCT ( 'Nut', 'Nut', '', ( #5253 ) ) ;
#5030 = CARTESIAN_POINT ( 'NONE',  ( 4.821444091131311524E-18, 0.1692468441617604180, 0.03937007874015747977 ) ) ;
#5031 = DIRECTION ( 'NONE',  ( 1.000000000000000000, 0.000000000000000000, 0.000000000000000000 ) ) ;
#5032 = CARTESIAN_POINT ( 'NONE',  ( -0.7455328141524870667, 1.338582677165354395, 0.3622425942647020669 ) ) ;
#5033 = CARTESIAN_POINT ( 'NONE',  ( -1.181102362204724310, 0.1240157480314959815, 0.02952755905511811330 ) ) ;
#5034 = CARTESIAN_POINT ( 'NONE',  ( 0.000000000000000000, 1.370078740157480546, 0.5984251968503937480 ) ) ;
#5035 = VERTEX_POINT ( 'NONE', #7171 ) ;
#5036 = ORIENTED_EDGE ( 'NONE', *, *, #1585, .F. ) ;
#5037 = EDGE_LOOP ( 'NONE', ( #13372, #9567, #1783, #8262 ) ) ;
#5038 = EDGE_CURVE ( 'NONE', #5966, #15216, #2473, .T. ) ;
#5039 = DIRECTION ( 'NONE',  ( 0.5000000000000004441, -7.511572993685840713E-15, 0.8660254037844384856 ) ) ;
#5040 = CARTESIAN_POINT ( 'NONE',  ( -1.943332415744267072, -2.937030685955435594, 0.01138609156041062685 ) ) ;
#5041 = DIRECTION ( 'NONE',  ( -0.000000000000000000, -0.000000000000000000, -1.000000000000000000 ) ) ;
#5042 = CARTESIAN_POINT ( 'NONE',  ( 1.141732283464566677, 4.044111181948214319E-16, 0.02559055118110236185 ) ) ;
#5043 = CYLINDRICAL_SURFACE ( 'NONE', #9141, 0.003937007874015749712 ) ;
#5044 = DIRECTION ( 'NONE',  ( 0.000000000000000000, -0.000000000000000000, 1.000000000000000000 ) ) ;
#5045 = DIRECTION ( 'NONE',  ( 0.000000000000000000, 0.000000000000000000, 1.000000000000000000 ) ) ;
#5046 = CARTESIAN_POINT ( 'NONE',  ( -1.938095037791507824, -2.767575974228406732, 0.1578476300086600059 ) ) ;
#5047 = DIRECTION ( 'NONE',  ( 0.4999999999999979461, 0.000000000000000000, 0.8660254037844398178 ) ) ;
#5048 = DIRECTION ( 'NONE',  ( 1.000000000000000000, 0.000000000000000000, 0.000000000000000000 ) ) ;
#5049 = VERTEX_POINT ( 'NONE', #48 ) ;
#5050 = VERTEX_POINT ( 'NONE', #7244 ) ;
#5051 = ORIENTED_EDGE ( 'NONE', *, *, #5670, .T. ) ;
#5052 = VERTEX_POINT ( 'NONE', #10483 ) ;
#5053 = ORIENTED_EDGE ( 'NONE', *, *, #10364, .T. ) ;
#5054 = FACE_OUTER_BOUND ( 'NONE', #11023, .T. ) ;
#5055 = LINE ( 'NONE', #2793, #14380 ) ;
#5056 = AXIS2_PLACEMENT_3D ( 'NONE', #231, #2779, #14482 ) ;
#5057 = AXIS2_PLACEMENT_3D ( 'NONE', #4764, #8360, #13063 ) ;
#5058 = EDGE_CURVE ( 'NONE', #877, #10762, #13433, .T. ) ;
#5059 = FACE_OUTER_BOUND ( 'NONE', #13105, .T. ) ;
#5060 = CARTESIAN_POINT ( 'NONE',  ( -1.181102362204724310, 0.000000000000000000, 0.02559055118110236185 ) ) ;
#5061 = TOROIDAL_SURFACE ( 'NONE', #13836, 0.04330708661417328326, 0.003937007874015747977 ) ;
#5062 = CARTESIAN_POINT ( 'NONE',  ( 0.06604848736013260724, 1.035433070866141891, -0.5868460571724354313 ) ) ;
#5063 = FACE_OUTER_BOUND ( 'NONE', #4814, .T. ) ;
#5064 = CARTESIAN_POINT ( 'NONE',  ( -1.883899324821880272, -2.911992577559399109, 0.05656501291315504942 ) ) ;
#5065 = EDGE_LOOP ( 'NONE', ( #4327, #12283 ) ) ;
#5066 = LINE ( 'NONE', #4222, #14450 ) ;
#5067 = FACE_OUTER_BOUND ( 'NONE', #3611, .T. ) ;
#5068 = CARTESIAN_POINT ( 'NONE',  ( -0.07874015748031501505, 0.1442356988431298948, -0.05905511811023622659 ) ) ;
#5069 = ORIENTED_EDGE ( 'NONE', *, *, #12584, .T. ) ;
#5070 = VERTEX_POINT ( 'NONE', #8132 ) ;
#5071 = CIRCLE ( 'NONE', #13843, 0.003937007874015741038 ) ;
#5072 = AXIS2_PLACEMENT_3D ( 'NONE', #6527, #5356, #3026 ) ;
#5073 = CIRCLE ( 'NONE', #7089, 0.003937007874015724558 ) ;
#5074 = AXIS2_PLACEMENT_3D ( 'NONE', #12648, #11477, #10754 ) ;
#5075 = ORIENTED_EDGE ( 'NONE', *, *, #1856, .F. ) ;
#5076 = EDGE_CURVE ( 'NONE', #10028, #14086, #14930, .T. ) ;
#5077 =( REPRESENTATION_RELATIONSHIP ('NONE','NONE', #8904, #12105 ) REPRESENTATION_RELATIONSHIP_WITH_TRANSFORMATION ( #14278 )SHAPE_REPRESENTATION_RELATIONSHIP( ) );
#5078 = ADVANCED_FACE ( 'NONE', ( #5690 ), #14116, .F. ) ;
#5079 = DIRECTION ( 'NONE',  ( -0.4999999999999919509, 0.000000000000000000, 0.8660254037844432595 ) ) ;
#5080 = DIRECTION ( 'NONE',  ( 1.000000000000000000, 0.000000000000000000, 0.000000000000000000 ) ) ;
#5081 = AXIS2_PLACEMENT_3D ( 'NONE', #7786, #5268, #13757 ) ;
#5082 = CARTESIAN_POINT ( 'NONE',  ( 0.06692913385832208184, -0.2952755905511811330, -0.4190977005962941426 ) ) ;
#5083 = AXIS2_PLACEMENT_3D ( 'NONE', #7388, #12187, #13206 ) ;
#5084 = CARTESIAN_POINT ( 'NONE',  ( -0.07635964791965739462, -0.1878198040935885327, -0.05905511811023622659 ) ) ;
#5085 = VERTEX_POINT ( 'NONE', #10837 ) ;
#5086 = DIRECTION ( 'NONE',  ( 1.000000000000000000, -0.000000000000000000, -0.000000000000000000 ) ) ;
#5087 = CIRCLE ( 'NONE', #13606, 0.003937007874015747109 ) ;
#5088 = DIRECTION ( 'NONE',  ( 1.000000000000000000, -0.000000000000000000, -0.000000000000000000 ) ) ;
#5089 = VECTOR ( 'NONE', #9498, 39.37007874015748143 ) ;
#5090 = DIRECTION ( 'NONE',  ( 0.000000000000000000, 0.000000000000000000, -1.000000000000000000 ) ) ;
#5091 = AXIS2_PLACEMENT_3D ( 'NONE', #1275, #9665, #7365 ) ;
#5092 = DIRECTION ( 'NONE',  ( -0.000000000000000000, 1.000000000000000000, 0.000000000000000000 ) ) ;
#5093 = B_SPLINE_CURVE_WITH_KNOTS ( 'NONE', 3,
 ( #10351, #13021, #6813, #10515, #5558, #9265 ),
 .UNSPECIFIED., .F., .F.,
 ( 4, 2, 4 ),
 ( -5.605548034552286995E-06, 0.0004410309859948809271, 0.0008876675200243141616 ),
 .UNSPECIFIED. ) ;
#5094 = DIRECTION ( 'NONE',  ( 1.224646799147353207E-16, 0.000000000000000000, -1.000000000000000000 ) ) ;
#5095 = ORIENTED_EDGE ( 'NONE', *, *, #10460, .F. ) ;
#5096 = EDGE_CURVE ( 'NONE', #14806, #7930, #12863, .T. ) ;
#5098 = VERTEX_POINT ( 'NONE', #1295 ) ;
#5097 = AXIS2_PLACEMENT_3D ( 'NONE', #14734, #310, #12227 ) ;
#5099 = AXIS2_PLACEMENT_3D ( 'NONE', #6276, #130, #7398 ) ;
#5100 = EDGE_CURVE ( 'NONE', #11872, #13296, #3793, .T. ) ;
#5101 = ORIENTED_EDGE ( 'NONE', *, *, #182, .F. ) ;
#5102 = CIRCLE ( 'NONE', #2860, 0.003937007874015741038 ) ;
#5103 = DIRECTION ( 'NONE',  ( 0.5000000000000004441, 0.000000000000000000, -0.8660254037844382635 ) ) ;
#5104 = CARTESIAN_POINT ( 'NONE',  ( 0.06299212598430634080, -0.4921259842519685179, -0.2366577558633030653 ) ) ;
#5105 = AXIS2_PLACEMENT_3D ( 'NONE', #4994, #3601, #14561 ) ;
#5106 = PRODUCT_DEFINITION_FORMATION_WITH_SPECIFIED_SOURCE ( 'ANY', '', #8171, .NOT_KNOWN. ) ;
#5107 = ADVANCED_FACE ( 'NONE', ( #14607 ), #11000, .T. ) ;
#5108 = CYLINDRICAL_SURFACE ( 'NONE', #12849, 0.003937007874015740171 ) ;
#5109 = CARTESIAN_POINT ( 'NONE',  ( 0.3137366569588399545, -0.2952755905511811330, 0.2947875711430715251 ) ) ;
#5110 = SHAPE_DEFINITION_REPRESENTATION ( #9430, #12705 ) ;
#5111 = DIRECTION ( 'NONE',  ( 0.8660254037844383745, -0.000000000000000000, 0.5000000000000002220 ) ) ;
#5112 = CARTESIAN_POINT ( 'NONE',  ( -0.1259842519685039353, 2.440944881889763884, 0.04724409448818898266 ) ) ;
#5113 = CARTESIAN_POINT ( 'NONE',  ( -0.1724006475077544398, -0.09842519685039370636, 0.1689446513984334541 ) ) ;
#5114 = DIRECTION ( 'NONE',  ( 0.5000000000000004441, 0.000000000000000000, -0.8660254037844382635 ) ) ;
#5115 = VECTOR ( 'NONE', #5654, 39.37007874015748143 ) ;
#5116 = AXIS2_PLACEMENT_3D ( 'NONE', #3546, #197, #7372 ) ;
#5117 = CIRCLE ( 'NONE', #1140, 0.5511811023622046335 ) ;
#5118 = DIRECTION ( 'NONE',  ( -1.000000000000000000, 0.000000000000000000, 0.000000000000000000 ) ) ;
#5119 = TOROIDAL_SURFACE ( 'NONE', #8896, 2.194881889763779181, 0.01968503937007873988 ) ;
#5120 = ORIENTED_EDGE ( 'NONE', *, *, #14129, .F. ) ;
#5121 = ORIENTED_EDGE ( 'NONE', *, *, #10213, .F. ) ;
#5122 = ORIENTED_EDGE ( 'NONE', *, *, #2713, .F. ) ;
#5123 = VECTOR ( 'NONE', #7993, 39.37007874015748143 ) ;
#5124 = CIRCLE ( 'NONE', #4636, 0.1279527559055117780 ) ;
#5125 = CIRCLE ( 'NONE', #3651, 0.003937007874015750579 ) ;
#5126 = DIRECTION ( 'NONE',  ( 1.060575238724907285E-16, 1.000000000000000000, -6.123233995736759873E-17 ) ) ;
#5127 = CARTESIAN_POINT ( 'NONE',  ( -1.946977922026294605, -2.928246735464111072, -0.08439612660844164616 ) ) ;
#5128 = CARTESIAN_POINT ( 'NONE',  ( -1.419615703680148000, -0.01226548409420231273, 0.07874015748031495954 ) ) ;
#5129 = EDGE_CURVE ( 'NONE', #11540, #4286, #9827, .T. ) ;
#5130 = AXIS2_PLACEMENT_3D ( 'NONE', #14735, #1722, #13848 ) ;
#5131 = CARTESIAN_POINT ( 'NONE',  ( 0.1618514667033794374, -0.09842519685039370636, 0.2161887458866224576 ) ) ;
#5132 = CARTESIAN_POINT ( 'NONE',  ( 0.4787089944775337336, 1.040121464703355425, 0.3474236500605593636 ) ) ;
#5133 = DIRECTION ( 'NONE',  ( 0.8180917953313872060, -0.5750876580239463465, 0.000000000000000000 ) ) ;
#5134 = CARTESIAN_POINT ( 'NONE',  ( -1.309055118110236116, 0.000000000000000000, 0.02952755905511811330 ) ) ;
#5135 = EDGE_CURVE ( 'NONE', #13899, #6200, #10055, .T. ) ;
#5136 = DIRECTION ( 'NONE',  ( 1.000000000000000000, 0.000000000000000000, -1.224646799147353207E-16 ) ) ;
#5137 = ADVANCED_FACE ( 'NONE', ( #8425 ), #12191, .F. ) ;
#5138 = CARTESIAN_POINT ( 'NONE',  ( 0.06440205152080440143, 1.344788853693112962, -0.5870313606185335598 ) ) ;
#5139 = PLANE ( 'NONE',  #10910 ) ;
#5140 = AXIS2_PLACEMENT_3D ( 'NONE', #12346, #3744, #11083 ) ;
#5141 = CIRCLE ( 'NONE', #13909, 0.5511811023622046335 ) ;
#5142 = EDGE_LOOP ( 'NONE', ( #4016, #12538, #9502, #9655 ) ) ;
#5143 = ORIENTED_EDGE ( 'NONE', *, *, #13797, .T. ) ;
#5144 = ORIENTED_EDGE ( 'NONE', *, *, #5004, .F. ) ;
#5145 = ORIENTED_EDGE ( 'NONE', *, *, #4242, .F. ) ;
#5146 = ORIENTED_EDGE ( 'NONE', *, *, #12303, .F. ) ;
#5147 = CARTESIAN_POINT ( 'NONE',  ( 0.05114323250695499562, 0.05905511811023622659, -0.08858267716535433989 ) ) ;
#5148 = DIRECTION ( 'NONE',  ( -0.000000000000000000, -1.000000000000000000, -0.000000000000000000 ) ) ;
#5149 = CARTESIAN_POINT ( 'NONE',  ( -0.1028896637645180384, -0.4881889763779528324, -0.2462933508112025438 ) ) ;
#5150 = CARTESIAN_POINT ( 'NONE',  ( -1.868497805385690214, -2.949470162837682707, 0.01421723262671847204 ) ) ;
#5151 = ORIENTED_EDGE ( 'NONE', *, *, #795, .F. ) ;
#5152 = CARTESIAN_POINT ( 'NONE',  ( 0.000000000000000000, 2.440944881889763884, 0.000000000000000000 ) ) ;
#5153 = CARTESIAN_POINT ( 'NONE',  ( 0.05905511811023625435, 2.637795275590551825, -0.03937007874015747977 ) ) ;
#5154 = CARTESIAN_POINT ( 'NONE',  ( -1.403645773789551576, -0.004863036735870162816, -0.05905511811023622659 ) ) ;
#5155 = ORIENTED_EDGE ( 'NONE', *, *, #12182, .F. ) ;
#5156 = ORIENTED_EDGE ( 'NONE', *, *, #11338, .T. ) ;
#5157 = CIRCLE ( 'NONE', #8943, 0.003937007874015780069 ) ;
#5158 = UNCERTAINTY_MEASURE_WITH_UNIT (LENGTH_MEASURE( 1.000000000000000082E-05 ), #9292, 'distance_accuracy_value', 'NONE');
#5159 = ORIENTED_EDGE ( 'NONE', *, *, #14082, .T. ) ;
#5160 = VECTOR ( 'NONE', #15124, 39.37007874015748143 ) ;
#5161 = DIRECTION ( 'NONE',  ( 1.000000000000000000, 0.000000000000000000, 0.000000000000000000 ) ) ;
#5162 = AXIS2_PLACEMENT_3D ( 'NONE', #1792, #15034, #15102 ) ;
#5164 = AXIS2_PLACEMENT_3D ( 'NONE', #3149, #7927, #10579 ) ;
#5163 = DIRECTION ( 'NONE',  ( 0.000000000000000000, 0.000000000000000000, -1.000000000000000000 ) ) ;
#5165 = CARTESIAN_POINT ( 'NONE',  ( -0.004461712539986224628, -0.1607679992104108779, -0.007865172455356563355 ) ) ;
#5166 = ORIENTED_EDGE ( 'NONE', *, *, #10276, .F. ) ;
#5167 = EDGE_CURVE ( 'NONE', #2172, #925, #8654, .T. ) ;
#5168 = DIRECTION ( 'NONE',  ( 1.000000000000000000, 0.000000000000000000, 0.000000000000000000 ) ) ;
#5169 = CARTESIAN_POINT ( 'NONE',  ( -0.09061599198715356018, 0.06736074103232447818, -0.007444810018878696839 ) ) ;
#5170 = DIRECTION ( 'NONE',  ( 1.000000000000000000, 0.000000000000000000, 0.000000000000000000 ) ) ;
#5171 = AXIS2_PLACEMENT_3D ( 'NONE', #3919, #11198, #4059 ) ;
#5172 = CARTESIAN_POINT ( 'NONE',  ( -0.4815353412745217998, 1.340095897400991110, 0.3474236500605538125 ) ) ;
#5173 = ADVANCED_FACE ( 'NONE', ( #3346 ), #10923, .T. ) ;
#5174 = CARTESIAN_POINT ( 'NONE',  ( -2.755905511811024056, -1.630597114118275348, 8.792486876640390747 ) ) ;
#5175 = ORIENTED_EDGE ( 'NONE', *, *, #7926, .F. ) ;
#5176 = ADVANCED_FACE ( 'NONE', ( #8798 ), #12634, .T. ) ;
#5177 = ORIENTED_EDGE ( 'NONE', *, *, #2996, .T. ) ;
#5178 = VECTOR ( 'NONE', #6767, 39.37007874015748143 ) ;
#5179 = EDGE_LOOP ( 'NONE', ( #1240, #11870 ) ) ;
#5180 = CARTESIAN_POINT ( 'NONE',  ( 0.000000000000000000, 1.385826771653543510, -0.7086614173228346081 ) ) ;
#5181 = FACE_OUTER_BOUND ( 'NONE', #7888, .T. ) ;
#5182 = TOROIDAL_SURFACE ( 'NONE', #8209, 0.1653543307086614012, 0.007874015748031495954 ) ;
#5183 = CARTESIAN_POINT ( 'NONE',  ( -0.05175539059627463218, 0.000000000000000000, 0.07475334604056275978 ) ) ;
#5184 = DIRECTION ( 'NONE',  ( 1.165734175856414170E-15, 0.5417705490259633327, 0.8405264256453250926 ) ) ;
#5185 = CARTESIAN_POINT ( 'NONE',  ( -0.01295353379695964903, 0.07061622514300590348, -0.08006968853231534455 ) ) ;
#5186 = CARTESIAN_POINT ( 'NONE',  ( -1.417802900492933782, -0.04287136159519133044, 0.07874015748031495954 ) ) ;
#5187 = EDGE_CURVE ( 'NONE', #6857, #15219, #7625, .T. ) ;
#5188 = FACE_OUTER_BOUND ( 'NONE', #3854, .T. ) ;
#5189 = DIRECTION ( 'NONE',  ( -3.645101222232083416E-12, -4.880852986322028827E-12, -1.000000000000000000 ) ) ;
#5190 = DIRECTION ( 'NONE',  ( -1.000000000000000000, 0.000000000000000000, -1.445602896647338424E-16 ) ) ;
#5191 = CIRCLE ( 'NONE', #968, 0.003937007874015724558 ) ;
#5192 = EDGE_CURVE ( 'NONE', #7138, #14594, #3636, .T. ) ;
#5193 = FACE_OUTER_BOUND ( 'NONE', #14322, .T. ) ;
#5194 = AXIS2_PLACEMENT_3D ( 'NONE', #12465, #1560, #14744 ) ;
#5195 = VERTEX_POINT ( 'NONE', #3955 ) ;
#5196 = EDGE_CURVE ( 'NONE', #14862, #7482, #15134, .T. ) ;
#5197 = FACE_OUTER_BOUND ( 'NONE', #8574, .T. ) ;
#5198 = ADVANCED_FACE ( 'NONE', ( #7773 ), #10220, .T. ) ;
#5199 = ORIENTED_EDGE ( 'NONE', *, *, #11637, .F. ) ;
#5200 = ORIENTED_EDGE ( 'NONE', *, *, #7107, .T. ) ;
#5201 = AXIS2_PLACEMENT_3D ( 'NONE', #541, #2887, #7742 ) ;
#5202 = FACE_OUTER_BOUND ( 'NONE', #502, .T. ) ;
#5203 = CARTESIAN_POINT ( 'NONE',  ( -1.947458820971768256, -2.927011135189118374, 0.05621523865303355155 ) ) ;
#5204 = CARTESIAN_POINT ( 'NONE',  ( 0.1618514667033794374, -0.1023622047244094474, 0.2161887458866224576 ) ) ;
#5205 = AXIS2_PLACEMENT_3D ( 'NONE', #10615, #4577, #11799 ) ;
#5206 = CARTESIAN_POINT ( 'NONE',  ( -0.5894146648244306119, -0.09448818897637796532, 0.1571437749735178357 ) ) ;
#5207 = DIRECTION ( 'NONE',  ( -0.000000000000000000, 1.000000000000000000, 0.000000000000000000 ) ) ;
#5208 = DIRECTION ( 'NONE',  ( -0.4999999999999966693, 0.000000000000000000, -0.8660254037844405950 ) ) ;
#5209 = CARTESIAN_POINT ( 'NONE',  ( 0.05175539059627461136, 0.07874015748031495954, -0.07475334604056278753 ) ) ;
#5210 = DIRECTION ( 'NONE',  ( -0.5000000000000001110, -0.000000000000000000, -0.8660254037844385966 ) ) ;
#5211 = CARTESIAN_POINT ( 'NONE',  ( -1.276200637803905691, -0.1988000726501942539, 0.1968503937007874127 ) ) ;
#5212 = DIRECTION ( 'NONE',  ( -0.000000000000000000, -2.212657494868377674E-16, 1.000000000000000000 ) ) ;
#5213 = EDGE_LOOP ( 'NONE', ( #7767, #2850, #1854, #15453, #15089, #10334, #4569, #40, #12072, #10045, #13787, #6908, #3109, #8223, #5069, #12985 ) ) ;
#5214 = ORIENTED_EDGE ( 'NONE', *, *, #7986, .F. ) ;
#5215 = EDGE_CURVE ( 'NONE', #6019, #12169, #5424, .T. ) ;
#5216 = VERTEX_POINT ( 'NONE', #12415 ) ;
#5217 = ORIENTED_EDGE ( 'NONE', *, *, #12254, .T. ) ;
#5218 = ORIENTED_EDGE ( 'NONE', *, *, #8555, .F. ) ;
#5219 = CARTESIAN_POINT ( 'NONE',  ( -1.387704745771440207, -0.02010536753476140082, -0.03937007874015747977 ) ) ;
#5220 = EDGE_CURVE ( 'NONE', #12883, #13266, #8380, .T. ) ;
#5221 = CARTESIAN_POINT ( 'NONE',  ( 0.03886060139087953863, 0.000000000000000000, 0.08219815605943972536 ) ) ;
#5222 = DIRECTION ( 'NONE',  ( 0.000000000000000000, 0.000000000000000000, -1.000000000000000000 ) ) ;
#5223 = CARTESIAN_POINT ( 'NONE',  ( 0.000000000000000000, 0.04724409448818898960, 0.000000000000000000 ) ) ;
#5224 = CARTESIAN_POINT ( 'NONE',  ( 0.1724006475077543565, -0.1023622047244094474, 0.1689446513984334541 ) ) ;
#5225 = CARTESIAN_POINT ( 'NONE',  ( 0.000000000000000000, 0.07874015748031495954, 0.04330708661417326938 ) ) ;
#5226 = PLANE ( 'NONE',  #2436 ) ;
#5227 = CARTESIAN_POINT ( 'NONE',  ( -1.868482444096062789, -2.949506639258173024, -0.006642451843458160692 ) ) ;
#5228 = ORIENTED_EDGE ( 'NONE', *, *, #998, .T. ) ;
#5229 = LINE ( 'NONE', #7511, #8945 ) ;
#5230 = DIRECTION ( 'NONE',  ( 0.000000000000000000, 1.000000000000000000, 0.000000000000000000 ) ) ;
#5231 = ORIENTED_EDGE ( 'NONE', *, *, #12228, .T. ) ;
#5232 = ORIENTED_EDGE ( 'NONE', *, *, #4068, .F. ) ;
#5233 = ORIENTED_EDGE ( 'NONE', *, *, #2028, .F. ) ;
#5234 = EDGE_CURVE ( 'NONE', #631, #6704, #911, .T. ) ;
#5235 = DIRECTION ( 'NONE',  ( -0.8660254037844405950, 0.000000000000000000, -0.4999999999999966693 ) ) ;
#5236 = DIRECTION ( 'NONE',  ( -0.000000000000000000, -1.000000000000000000, -0.000000000000000000 ) ) ;
#5237 = FACE_BOUND ( 'NONE', #11484, .T. ) ;
#5238 = EDGE_LOOP ( 'NONE', ( #14060, #5771, #989 ) ) ;
#5239 = FACE_OUTER_BOUND ( 'NONE', #734, .T. ) ;
#5240 = FACE_BOUND ( 'NONE', #15419, .T. ) ;
#5241 = DIRECTION ( 'NONE',  ( 0.000000000000000000, 0.000000000000000000, 1.000000000000000000 ) ) ;
#5242 = CARTESIAN_POINT ( 'NONE',  ( -0.09842519685028333631, -0.2952755905511811330, -0.4584677793364517195 ) ) ;
#5243 = B_SPLINE_CURVE_WITH_KNOTS ( 'NONE', 3,
 ( #13390, #244, #6083, #14330, #1414, #8378, #13164, #1257 ),
 .UNSPECIFIED., .F., .F.,
 ( 4, 2, 2, 4 ),
 ( 0.000000000000000000, 0.0004641946399066459767, 0.0009283892798132919533, 0.001856778559626583907 ),
 .UNSPECIFIED. ) ;
#5244 = LINE ( 'NONE', #11973, #2834 ) ;
#5245 = DIRECTION ( 'NONE',  ( 0.000000000000000000, 0.000000000000000000, -1.000000000000000000 ) ) ;
#5246 = VERTEX_POINT ( 'NONE', #3074 ) ;
#5247 = ORIENTED_EDGE ( 'NONE', *, *, #3938, .F. ) ;
#5248 = VERTEX_POINT ( 'NONE', #5186 ) ;
#5249 = DIRECTION ( 'NONE',  ( 0.000000000000000000, 0.000000000000000000, -1.000000000000000000 ) ) ;
#5250 = EDGE_CURVE ( 'NONE', #4540, #11532, #2935, .T. ) ;
#5251 = CARTESIAN_POINT ( 'NONE',  ( -2.080881322745466999, -1.632190302820504257, 0.08366141732283423338 ) ) ;
#5252 = DIRECTION ( 'NONE',  ( -0.5000000000000209832, -0.000000000000000000, -0.8660254037844266062 ) ) ;
#5253 = PRODUCT_CONTEXT ( 'NONE', #1104, 'mechanical' ) ;
#5254 = CYLINDRICAL_SURFACE ( 'NONE', #2847, 0.5905511811023621549 ) ;
#5255 = CARTESIAN_POINT ( 'NONE',  ( -0.7455328141524873997, 1.043307086614173151, 0.3622425942647021779 ) ) ;
#5256 = CARTESIAN_POINT ( 'NONE',  ( 0.4749369078591172966, -0.4881889763779528324, 0.3514880584999470203 ) ) ;
#5257 = EDGE_CURVE ( 'NONE', #12689, #13984, #4113, .T. ) ;
#5258 = FACE_OUTER_BOUND ( 'NONE', #9608, .T. ) ;
#5259 = CARTESIAN_POINT ( 'NONE',  ( -0.2362204724409448231, -0.02638708502139245488, -0.03937007874015747977 ) ) ;
#5260 = CARTESIAN_POINT ( 'NONE',  ( -0.4625984251968516259, -0.4881889763779528324, 0.3807329531073311846 ) ) ;
#5261 = ORIENTED_EDGE ( 'NONE', *, *, #6147, .F. ) ;
#5262 = EDGE_LOOP ( 'NONE', ( #15135, #10752, #11575, #2964 ) ) ;
#5263 = CARTESIAN_POINT ( 'NONE',  ( -0.5412478373021294420, 1.035433070866141891, 0.2362233606508100381 ) ) ;
#5264 = ORIENTED_EDGE ( 'NONE', *, *, #8307, .T. ) ;
#5265 = ORIENTED_EDGE ( 'NONE', *, *, #12761, .F. ) ;
#5266 = EDGE_CURVE ( 'NONE', #2421, #6774, #15002, .T. ) ;
#5267 = EDGE_CURVE ( 'NONE', #12909, #4631, #11233, .T. ) ;
#5268 = DIRECTION ( 'NONE',  ( -0.5801894994542525774, -0.8144815189573204606, 0.000000000000000000 ) ) ;
#5269 = CARTESIAN_POINT ( 'NONE',  ( -1.938169220489598832, -2.949504990652386027, 0.006020211170025131266 ) ) ;
#5270 = SHAPE_REPRESENTATION_RELATIONSHIP ( 'NONE' , 'NONE' ,  #11075, #11164 ) ;
#5271 = CARTESIAN_POINT ( 'NONE',  ( -0.4625984251968516259, -0.1023622047244094474, 0.3807329531073311846 ) ) ;
#5272 = EDGE_CURVE ( 'NONE', #11465, #15025, #14379, .T. ) ;
#5273 = CARTESIAN_POINT ( 'NONE',  ( -1.997526618581371816, -2.796735537175909503, -0.1565704719341493578 ) ) ;
#5274 = FACE_OUTER_BOUND ( 'NONE', #9737, .T. ) ;
#5275 = DIRECTION ( 'NONE',  ( 0.000000000000000000, 0.000000000000000000, 1.000000000000000000 ) ) ;
#5276 = CARTESIAN_POINT ( 'NONE',  ( -1.904797909729390337, -2.859137677581157000, 0.1269363942893919350 ) ) ;
#5277 = DIRECTION ( 'NONE',  ( 0.4999999999999966693, 0.000000000000000000, -0.8660254037844405950 ) ) ;
#5278 = ORIENTED_EDGE ( 'NONE', *, *, #10784, .T. ) ;
#5279 = ORIENTED_EDGE ( 'NONE', *, *, #5473, .T. ) ;
#5280 = EDGE_LOOP ( 'NONE', ( #2828, #696 ) ) ;
#5281 = VERTEX_POINT ( 'NONE', #10052 ) ;
#5282 = EDGE_CURVE ( 'NONE', #697, #2543, #14834, .T. ) ;
#5283 = ORIENTED_EDGE ( 'NONE', *, *, #8253, .F. ) ;
#5284 = EDGE_CURVE ( 'NONE', #10725, #675, #14767, .T. ) ;
#5285 = CARTESIAN_POINT ( 'NONE',  ( -1.406483596012642945, -0.03325901290046209824, -0.04682391966548175855 ) ) ;
#5286 = CYLINDRICAL_SURFACE ( 'NONE', #2331, 0.003937007874015754916 ) ;
#5287 = DIRECTION ( 'NONE',  ( -0.000000000000000000, -0.000000000000000000, -1.000000000000000000 ) ) ;
#5288 = DIRECTION ( 'NONE',  ( 3.614007241618347785E-16, -0.000000000000000000, -1.000000000000000000 ) ) ;
#5289 = CARTESIAN_POINT ( 'NONE',  ( 0.4765664223159776780, 1.344138844425384560, 0.3487699017371386212 ) ) ;
#5290 = EDGE_CURVE ( 'NONE', #15055, #3552, #7708, .T. ) ;
#5291 = CARTESIAN_POINT ( 'NONE',  ( -0.1552072824047652788, -0.09842519685039370636, -0.5870514566507987197 ) ) ;
#5292 = CARTESIAN_POINT ( 'NONE',  ( -1.181096721695571894, 0.3434326084030802084, 0.04453596627282299658 ) ) ;
#5293 = CARTESIAN_POINT ( 'NONE',  ( -1.877572016762099727, -2.927690193651851569, 0.08555793721333695978 ) ) ;
#5294 = ORIENTED_EDGE ( 'NONE', *, *, #7781, .F. ) ;
#5295 = DIRECTION ( 'NONE',  ( -0.000000000000000000, -1.000000000000000000, -0.000000000000000000 ) ) ;
#5296 = DIRECTION ( 'NONE',  ( 0.000000000000000000, 0.000000000000000000, -1.000000000000000000 ) ) ;
#5297 = DIRECTION ( 'NONE',  ( 1.000000000000000000, 0.000000000000000000, 0.000000000000000000 ) ) ;
#5298 = ORIENTED_EDGE ( 'NONE', *, *, #11437, .T. ) ;
#5299 = ADVANCED_FACE ( 'NONE', ( #1522 ), #6274, .T. ) ;
#5300 = ORIENTED_EDGE ( 'NONE', *, *, #3571, .T. ) ;
#5301 = EDGE_LOOP ( 'NONE', ( #3943, #9757, #10992, #5655 ) ) ;
#5302 = AXIS2_PLACEMENT_3D ( 'NONE', #8221, #1014, #10639 ) ;
#5303 = VECTOR ( 'NONE', #6943, 39.37007874015748143 ) ;
#5304 = DIRECTION ( 'NONE',  ( -0.5000000000000001110, 0.000000000000000000, -0.8660254037844384856 ) ) ;
#5305 = CARTESIAN_POINT ( 'NONE',  ( -0.3294846884549020305, -0.2952755905511811330, 0.2675111804726948983 ) ) ;
#5306 = EDGE_CURVE ( 'NONE', #2107, #12371, #13890, .T. ) ;
#5307 = DIRECTION ( 'NONE',  ( -0.000000000000000000, 1.000000000000000000, 0.000000000000000000 ) ) ;
#5308 = CARTESIAN_POINT ( 'NONE',  ( -0.06762554849860662187, -0.1867557816141671156, -0.05879187219561133465 ) ) ;
#5309 = ORIENTED_EDGE ( 'NONE', *, *, #14781, .F. ) ;
#5310 = CARTESIAN_POINT ( 'NONE',  ( 0.2647411304680618027, -0.4881889763779528324, 0.03404161279868787859 ) ) ;
#5311 = CARTESIAN_POINT ( 'NONE',  ( -0.5068643957866975081, 1.043307086614173373, 0.2244473186741497150 ) ) ;
#5312 = VECTOR ( 'NONE', #6476, 39.37007874015748143 ) ;
#5313 = AXIS2_PLACEMENT_3D ( 'NONE', #8989, #4118, #5208 ) ;
#5314 = CARTESIAN_POINT ( 'NONE',  ( -1.415033785308578818, -0.04025034750195270045, -0.05842314581460250622 ) ) ;
#5315 = EDGE_CURVE ( 'NONE', #253, #15013, #6751, .T. ) ;
#5316 = DIRECTION ( 'NONE',  ( -1.060575238724908024E-16, -0.4999999999999979461, -0.8660254037844397068 ) ) ;
#5317 = CIRCLE ( 'NONE', #3334, 0.01968503937007874682 ) ;
#5318 = EDGE_CURVE ( 'NONE', #14839, #8213, #11120, .T. ) ;
#5319 = CARTESIAN_POINT ( 'NONE',  ( -1.137795275590550936, 0.000000000000000000, -0.02952755905511811330 ) ) ;
#5320 = AXIS2_PLACEMENT_3D ( 'NONE', #10541, #4218, #11339 ) ;
#5321 = VERTEX_POINT ( 'NONE', #5797 ) ;
#5322 = EDGE_LOOP ( 'NONE', ( #1267, #8169, #7556, #3508 ) ) ;
#5323 = ORIENTED_EDGE ( 'NONE', *, *, #14749, .T. ) ;
#5324 = LINE ( 'NONE', #6266, #168 ) ;
#5325 = DIRECTION ( 'NONE',  ( 0.5000000000000001110, 0.000000000000000000, -0.8660254037844385966 ) ) ;
#5326 = VECTOR ( 'NONE', #14710, 39.37007874015748143 ) ;
#5327 = CIRCLE ( 'NONE', #2587, 0.7086614173228346081 ) ;
#5328 = VECTOR ( 'NONE', #14575, 39.37007874015748143 ) ;
#5329 = CARTESIAN_POINT ( 'NONE',  ( 6.846450609406462919E-17, 0.3543307086614172485, 0.5590551181102362266 ) ) ;
#5330 = DIRECTION ( 'NONE',  ( 0.000000000000000000, -1.000000000000000000, -0.000000000000000000 ) ) ;
#5331 = CIRCLE ( 'NONE', #3348, 0.1614173228346456879 ) ;
#5332 = APPLICATION_PROTOCOL_DEFINITION ( 'draft international standard', 'automotive_design', 1998, #8095 ) ;
#5333 = DIRECTION ( 'NONE',  ( -1.000000000000000000, 0.000000000000000000, 0.000000000000000000 ) ) ;
#5334 = CARTESIAN_POINT ( 'NONE',  ( 0.4342073824196633347, -0.09842519685039370636, 0.4299076816772810505 ) ) ;
#5335 = DIRECTION ( 'NONE',  ( 0.7402970580929290056, 0.6722799013647177135, 1.457774659155935170E-16 ) ) ;
#5336 = DIRECTION ( 'NONE',  ( 0.000000000000000000, 0.000000000000000000, -1.000000000000000000 ) ) ;
#5337 = LINE ( 'NONE', #3010, #11121 ) ;
#5338 = DIRECTION ( 'NONE',  ( -1.000000000000000000, 0.000000000000000000, 0.000000000000000000 ) ) ;
#5339 = AXIS2_PLACEMENT_3D ( 'NONE', #2093, #14878, #13706 ) ;
#5340 = AXIS2_PLACEMENT_3D ( 'NONE', #9110, #5649, #9036 ) ;
#5341 = ORIENTED_EDGE ( 'NONE', *, *, #10108, .T. ) ;
#5342 = TOROIDAL_SURFACE ( 'NONE', #7353, 0.04330708661417329020, 0.003937007874015747977 ) ;
#5343 = DIRECTION ( 'NONE',  ( 0.5000000000000004441, -0.000000000000000000, -0.8660254037844383745 ) ) ;
#5344 = VECTOR ( 'NONE', #14191, 39.37007874015748143 ) ;
#5345 = VERTEX_POINT ( 'NONE', #6995 ) ;
#5346 = ORIENTED_EDGE ( 'NONE', *, *, #13764, .T. ) ;
#5347 = AXIS2_PLACEMENT_3D ( 'NONE', #212, #14297, #10768 ) ;
#5348 = CARTESIAN_POINT ( 'NONE',  ( -0.09842519685028340570, -0.1023622047244094474, -0.5909884645248143498 ) ) ;
#5349 = CARTESIAN_POINT ( 'NONE',  ( -1.950663589855595736, -2.877608764542115782, 0.1430332175041234555 ) ) ;
#5350 = AXIS2_PLACEMENT_3D ( 'NONE', #6210, #3728, #7472 ) ;
#5351 = CIRCLE ( 'NONE', #9384, 0.003937007874015724558 ) ;
#5352 = CIRCLE ( 'NONE', #6361, 0.003937007874015749712 ) ;
#5353 = CARTESIAN_POINT ( 'NONE',  ( -0.4307978335858689278, -0.09842519685039370636, 0.4279391777402706265 ) ) ;
#5354 = VECTOR ( 'NONE', #10495, 39.37007874015748143 ) ;
#5355 = CARTESIAN_POINT ( 'NONE',  ( -1.983835277982623380, -2.834152059666824375, -0.1479904830673641758 ) ) ;
#5356 = DIRECTION ( 'NONE',  ( -1.000000000000000000, 0.000000000000000000, 0.000000000000000000 ) ) ;
#5357 = TOROIDAL_SURFACE ( 'NONE', #2363, 0.04330708661417328326, 0.003937007874015747977 ) ;
#5358 = CARTESIAN_POINT ( 'NONE',  ( 0.1618514667033794652, -0.1023622047244094474, 0.2161887458866224576 ) ) ;
#5359 = EDGE_CURVE ( 'NONE', #105, #10242, #11738, .T. ) ;
#5360 = EDGE_CURVE ( 'NONE', #9606, #12240, #3733, .T. ) ;
#5361 = DIRECTION ( 'NONE',  ( -0.000000000000000000, -1.000000000000000000, -0.000000000000000000 ) ) ;
#5362 = DIRECTION ( 'NONE',  ( -0.000000000000000000, 1.000000000000000000, 0.000000000000000000 ) ) ;
#5363 = ADVANCED_FACE ( 'NONE', ( #2222 ), #15064, .F. ) ;
#5364 = ORIENTED_EDGE ( 'NONE', *, *, #708, .T. ) ;
#5365 = ORIENTED_EDGE ( 'NONE', *, *, #9953, .T. ) ;
#5366 = AXIS2_PLACEMENT_3D ( 'NONE', #12711, #13954, #4233 ) ;
#5367 = ORIENTED_EDGE ( 'NONE', *, *, #1764, .F. ) ;
#5368 = CIRCLE ( 'NONE', #9398, 0.003937007874015750579 ) ;
#5369 = AXIS2_PLACEMENT_3D ( 'NONE', #11117, #2608, #13338 ) ;
#5370 = ORIENTED_EDGE ( 'NONE', *, *, #14763, .T. ) ;
#5371 = EDGE_CURVE ( 'NONE', #11768, #517, #13881, .T. ) ;
#5372 = ORIENTED_EDGE ( 'NONE', *, *, #4271, .T. ) ;
#5373 = CIRCLE ( 'NONE', #2876, 0.01968503937007880233 ) ;
#5374 = CARTESIAN_POINT ( 'NONE',  ( 0.000000000000000000, 1.645669291338583085, 0.000000000000000000 ) ) ;
#5375 = DIRECTION ( 'NONE',  ( 0.000000000000000000, 0.000000000000000000, 1.000000000000000000 ) ) ;
#5376 = CYLINDRICAL_SURFACE ( 'NONE', #15391, 0.03937007874015747977 ) ;
#5377 = CARTESIAN_POINT ( 'NONE',  ( -2.184126211765464287, -1.725292181286298021, 0.08417626406393743932 ) ) ;
#5378 = DIRECTION ( 'NONE',  ( -0.5692328345973325376, 0.000000000000000000, 0.8221763679505059708 ) ) ;
#5379 = DIRECTION ( 'NONE',  ( 0.000000000000000000, 0.000000000000000000, 1.000000000000000000 ) ) ;
#5380 = DIRECTION ( 'NONE',  ( 1.000000000000000000, 0.000000000000000000, -1.224646799147353207E-16 ) ) ;
#5381 = AXIS2_PLACEMENT_3D ( 'NONE', #11057, #7531, #1586 ) ;
#5382 = CARTESIAN_POINT ( 'NONE',  ( -1.182069932165816351, 0.3415656170894307286, 0.04962985469508127828 ) ) ;
#5383 = CIRCLE ( 'NONE', #3151, 0.003937007874015724558 ) ;
#5384 = FACE_OUTER_BOUND ( 'NONE', #9295, .T. ) ;
#5385 = AXIS2_PLACEMENT_3D ( 'NONE', #8312, #6910, #6746 ) ;
#5386 = ORIENTED_EDGE ( 'NONE', *, *, #1148, .F. ) ;
#5387 = CARTESIAN_POINT ( 'NONE',  ( -1.992382107315056716, -2.749515453455444902, -0.1756903148397133130 ) ) ;
#5388 = ADVANCED_FACE ( 'NONE', ( #4488 ), #5498, .T. ) ;
#5389 = CIRCLE ( 'NONE', #7399, 0.7086614173228346081 ) ;
#5390 = EDGE_CURVE ( 'NONE', #9996, #14180, #4647, .T. ) ;
#5392 = ORIENTED_EDGE ( 'NONE', *, *, #13235, .T. ) ;
#5391 =( REPRESENTATION_RELATIONSHIP ('NONE','NONE', #8904, #7785 ) REPRESENTATION_RELATIONSHIP_WITH_TRANSFORMATION ( #11851 )SHAPE_REPRESENTATION_RELATIONSHIP( ) );
#5393 = ORIENTED_EDGE ( 'NONE', *, *, #14484, .T. ) ;
#5394 = EDGE_CURVE ( 'NONE', #11324, #15288, #13135, .T. ) ;
#5396 = EDGE_LOOP ( 'NONE', ( #6986, #5465, #14721, #8520 ) ) ;
#5395 = AXIS2_PLACEMENT_3D ( 'NONE', #15139, #13740, #2134 ) ;
#5397 = AXIS2_PLACEMENT_3D ( 'NONE', #5749, #8339, #15325 ) ;
#5398 = AXIS2_PLACEMENT_3D ( 'NONE', #2143, #7942, #1992 ) ;
#5399 = B_SPLINE_CURVE_WITH_KNOTS ( 'NONE', 3,
 ( #9024, #2915, #10120, #728 ),
 .UNSPECIFIED., .F., .F.,
 ( 4, 4 ),
 ( 0.000000000000000000, 2.119993237936300859E-05 ),
 .UNSPECIFIED. ) ;
#5400 = CARTESIAN_POINT ( 'NONE',  ( -0.4828087445803670441, 1.042547362667152644, 0.3474236500605482614 ) ) ;
#5401 = PLANE ( 'NONE',  #11732 ) ;
#5402 = DIRECTION ( 'NONE',  ( -0.5000000000000035527, -0.000000000000000000, 0.8660254037844365982 ) ) ;
#5403 = ORIENTED_EDGE ( 'NONE', *, *, #12241, .F. ) ;
#5404 = CARTESIAN_POINT ( 'NONE',  ( -0.06351958502436047538, -0.4881889763779528324, -0.2357441700068276802 ) ) ;
#5405 = CARTESIAN_POINT ( 'NONE',  ( 0.000000000000000000, 0.000000000000000000, 0.000000000000000000 ) ) ;
#5406 = AXIS2_PLACEMENT_3D ( 'NONE', #10368, #11624, #14217 ) ;
#5407 = CARTESIAN_POINT ( 'NONE',  ( -1.417802900492933782, -0.04287136159519135820, -0.07874015748031495954 ) ) ;
#5408 = DIRECTION ( 'NONE',  ( -0.000000000000000000, -0.000000000000000000, -1.000000000000000000 ) ) ;
#5409 = ORIENTED_EDGE ( 'NONE', *, *, #2027, .T. ) ;
#5410 = FACE_OUTER_BOUND ( 'NONE', #10674, .T. ) ;
#5411 = CIRCLE ( 'NONE', #3926, 0.003937007874015749712 ) ;
#5412 = ORIENTED_EDGE ( 'NONE', *, *, #14823, .F. ) ;
#5413 = EDGE_CURVE ( 'NONE', #13551, #6722, #2141, .T. ) ;
#5414 = ORIENTED_EDGE ( 'NONE', *, *, #13630, .F. ) ;
#5415 = ORIENTED_EDGE ( 'NONE', *, *, #1773, .F. ) ;
#5416 = CARTESIAN_POINT ( 'NONE',  ( -1.491640810881974755, 0.2222636556240916161, 0.05905511811023622659 ) ) ;
#5417 = LINE ( 'NONE', #6667, #7156 ) ;
#5418 = VECTOR ( 'NONE', #11952, 39.37007874015748143 ) ;
#5419 = ADVANCED_FACE ( 'NONE', ( #14126 ), #12956, .T. ) ;
#5420 = CARTESIAN_POINT ( 'NONE',  ( -0.004867930653580591037, 0.1761271985362268533, -0.009096853601410393939 ) ) ;
#5421 = DIRECTION ( 'NONE',  ( 0.5000000000000033307, 4.518412553833339729E-17, -0.8660254037844365982 ) ) ;
#5422 = CARTESIAN_POINT ( 'NONE',  ( -0.02952755905509086426, -0.09842519685039370636, -0.05114323250690790829 ) ) ;
#5423 = TOROIDAL_SURFACE ( 'NONE', #7679, 0.5590551181102362266, 0.007874015748031495954 ) ;
#5424 = LINE ( 'NONE', #2841, #5856 ) ;
#5425 = EDGE_LOOP ( 'NONE', ( #13576, #12089, #1146, #1960, #4000, #14760 ) ) ;
#5426 = DIRECTION ( 'NONE',  ( 0.5000000000000037748, -0.000000000000000000, 0.8660254037844365982 ) ) ;
#5427 = DIRECTION ( 'NONE',  ( 0.4999999999999966693, 0.000000000000000000, -0.8660254037844405950 ) ) ;
#5428 = AXIS2_PLACEMENT_3D ( 'NONE', #14186, #1191, #3455 ) ;
#5429 = DIRECTION ( 'NONE',  ( 0.000000000000000000, 0.000000000000000000, 1.000000000000000000 ) ) ;
#5430 = CARTESIAN_POINT ( 'NONE',  ( -1.181102362204724310, 0.1279527559055117225, -0.02559055118110236185 ) ) ;
#5431 = ORIENTED_EDGE ( 'NONE', *, *, #15304, .T. ) ;
#5432 = AXIS2_PLACEMENT_3D ( 'NONE', #4362, #11189, #5222 ) ;
#5433 = ORIENTED_EDGE ( 'NONE', *, *, #3245, .T. ) ;
#5434 = SPHERICAL_SURFACE ( 'NONE', #14135, 0.003937007874015747977 ) ;
#5435 = ORIENTED_EDGE ( 'NONE', *, *, #4359, .F. ) ;
#5436 = CIRCLE ( 'NONE', #8445, 0.007874015748031504627 ) ;
#5437 = ORIENTED_EDGE ( 'NONE', *, *, #2408, .F. ) ;
#5438 = EDGE_CURVE ( 'NONE', #11495, #6564, #7360, .T. ) ;
#5439 = DIRECTION ( 'NONE',  ( -0.8660254037844388186, 0.000000000000000000, 0.4999999999999998335 ) ) ;
#5440 = CARTESIAN_POINT ( 'NONE',  ( -1.978999946204262006, -2.792301496701129704, 0.1761415058630058927 ) ) ;
#5441 = DIRECTION ( 'NONE',  ( 1.000000000000000000, 0.000000000000000000, 0.000000000000000000 ) ) ;
#5442 = AXIS2_PLACEMENT_3D ( 'NONE', #755, #2778, #685 ) ;
#5443 = FACE_OUTER_BOUND ( 'NONE', #6894, .T. ) ;
#5444 = DIRECTION ( 'NONE',  ( 0.000000000000000000, 0.000000000000000000, 1.000000000000000000 ) ) ;
#5445 = CARTESIAN_POINT ( 'NONE',  ( 0.000000000000000000, 0.000000000000000000, -0.6692913385826770867 ) ) ;
#5446 = AXIS2_PLACEMENT_3D ( 'NONE', #7440, #9565, #13173 ) ;
#5447 = FACE_OUTER_BOUND ( 'NONE', #470, .T. ) ;
#5448 = DIRECTION ( 'NONE',  ( -0.5000000000000035527, 0.000000000000000000, 0.8660254037844365982 ) ) ;
#5449 = LINE ( 'NONE', #12517, #12660 ) ;
#5450 = ORIENTED_EDGE ( 'NONE', *, *, #1388, .F. ) ;
#5451 = EDGE_LOOP ( 'NONE', ( #12154, #5365, #3191, #8245 ) ) ;
#5452 = AXIS2_PLACEMENT_3D ( 'NONE', #14025, #4387, #10734 ) ;
#5453 = ORIENTED_EDGE ( 'NONE', *, *, #4125, .F. ) ;
#5454 = ORIENTED_EDGE ( 'NONE', *, *, #6336, .F. ) ;
#5455 = AXIS2_PLACEMENT_3D ( 'NONE', #227, #5041, #9842 ) ;
#5456 = CARTESIAN_POINT ( 'NONE',  ( 0.01295353379695985026, 0.07061622514300630593, 0.08006968853231406780 ) ) ;
#5457 = PLANE ( 'NONE',  #11376 ) ;
#5458 = EDGE_CURVE ( 'NONE', #2367, #11305, #7852, .T. ) ;
#5459 = DIRECTION ( 'NONE',  ( 0.000000000000000000, 0.000000000000000000, 1.000000000000000000 ) ) ;
#5460 = CARTESIAN_POINT ( 'NONE',  ( 7.135737254874341425E-17, 2.433070866141732846, 0.5826771653543306728 ) ) ;
#5461 = DIRECTION ( 'NONE',  ( 0.8660254037844431485, -4.956352788505159323E-16, 0.4999999999999918954 ) ) ;
#5462 = LINE ( 'NONE', #8110, #15088 ) ;
#5463 = CARTESIAN_POINT ( 'NONE',  ( -1.180847381051831180, 0.3433074774307591781, 0.03937007874014957637 ) ) ;
#5464 = CYLINDRICAL_SURFACE ( 'NONE', #1152, 0.01968503937007875723 ) ;
#5465 = ORIENTED_EDGE ( 'NONE', *, *, #752, .F. ) ;
#5466 = DIRECTION ( 'NONE',  ( 0.5000000000000004441, -1.162044386198250571E-15, -0.8660254037844384856 ) ) ;
#5467 = EDGE_CURVE ( 'NONE', #5735, #10243, #6360, .T. ) ;
#5468 = CARTESIAN_POINT ( 'NONE',  ( -0.5445274672588088505, 1.338626482899105241, 0.2461921031270815630 ) ) ;
#5469 = EDGE_LOOP ( 'NONE', ( #632, #3017, #3905, #1331 ) ) ;
#5470 = ORIENTED_EDGE ( 'NONE', *, *, #14303, .T. ) ;
#5471 = ORIENTED_EDGE ( 'NONE', *, *, #11123, .F. ) ;
#5472 = DIRECTION ( 'NONE',  ( 0.000000000000000000, -0.000000000000000000, 1.000000000000000000 ) ) ;
#5473 = EDGE_CURVE ( 'NONE', #6948, #12093, #5768, .T. ) ;
#5474 = ADVANCED_FACE ( 'NONE', ( #5724 ), #6674, .F. ) ;
#5475 = DIRECTION ( 'NONE',  ( -0.5000000000000004441, 0.000000000000000000, 0.8660254037844384856 ) ) ;
#5476 = CARTESIAN_POINT ( 'NONE',  ( -0.4859532342797812654, 1.043307086614173373, 0.3487562073009442543 ) ) ;
#5477 = DIRECTION ( 'NONE',  ( -0.000000000000000000, -1.000000000000000000, -0.000000000000000000 ) ) ;
#5478 = FACE_OUTER_BOUND ( 'NONE', #7497, .T. ) ;
#5479 = LINE ( 'NONE', #6731, #5123 ) ;
#5480 = ORIENTED_EDGE ( 'NONE', *, *, #1184, .T. ) ;
#5481 = CARTESIAN_POINT ( 'NONE',  ( -2.026798844142627676, -2.454534756249174166, 0.1228056342163675041 ) ) ;
#5482 = ADVANCED_FACE ( 'NONE', ( #2364 ), #3708, .F. ) ;
#5483 = FACE_OUTER_BOUND ( 'NONE', #2943, .T. ) ;
#5484 = FACE_OUTER_BOUND ( 'NONE', #10149, .T. ) ;
#5485 = DIRECTION ( 'NONE',  ( 0.000000000000000000, -1.000000000000000000, 0.000000000000000000 ) ) ;
#5486 = VERTEX_POINT ( 'NONE', #9747 ) ;
#5487 = SURFACE_STYLE_USAGE ( .BOTH. , #500 ) ;
#5488 = ORIENTED_EDGE ( 'NONE', *, *, #15357, .T. ) ;
#5489 = ORIENTED_EDGE ( 'NONE', *, *, #11299, .F. ) ;
#5490 = EDGE_LOOP ( 'NONE', ( #10349, #1332, #14883, #6365, #3047 ) ) ;
#5491 = LINE ( 'NONE', #12861, #12173 ) ;
#5492 = LINE ( 'NONE', #14996, #6635 ) ;
#5493 = EDGE_CURVE ( 'NONE', #2210, #6005, #9668, .T. ) ;
#5494 = DIRECTION ( 'NONE',  ( 0.8660254037844385966, 0.000000000000000000, 0.5000000000000001110 ) ) ;
#5495 = DIRECTION ( 'NONE',  ( 0.000000000000000000, -1.000000000000000000, 0.000000000000000000 ) ) ;
#5496 = ITEM_DEFINED_TRANSFORMATION ( 'NONE', 'NONE', #8121,  #11481 ) ;
#5497 = FACE_OUTER_BOUND ( 'NONE', #7818, .T. ) ;
#5498 = CYLINDRICAL_SURFACE ( 'NONE', #9632, 0.003937007874015758385 ) ;
#5499 = ORIENTED_EDGE ( 'NONE', *, *, #2878, .T. ) ;
#5500 = CARTESIAN_POINT ( 'NONE',  ( -2.184126211765464287, -1.725292181286280258, -0.08417626406393655114 ) ) ;
#5501 = EDGE_CURVE ( 'NONE', #161, #4794, #10684, .T. ) ;
#5502 = PLANE ( 'NONE',  #382 ) ;
#5503 = DIRECTION ( 'NONE',  ( -0.5000000000000069944, -0.000000000000000000, -0.8660254037844347108 ) ) ;
#5504 = B_SPLINE_CURVE_WITH_KNOTS ( 'NONE', 3,
 ( #5550, #12683, #11265, #2882, #7808, #5377 ),
 .UNSPECIFIED., .F., .F.,
 ( 4, 2, 4 ),
 ( 0.000000000000000000, 0.01333398518358727691, 0.02666797036717455383 ),
 .UNSPECIFIED. ) ;
#5505 = ORIENTED_EDGE ( 'NONE', *, *, #12507, .F. ) ;
#5506 = EDGE_CURVE ( 'NONE', #14774, #13179, #8621, .T. ) ;
#5507 = FACE_OUTER_BOUND ( 'NONE', #12554, .T. ) ;
#5508 = ORIENTED_EDGE ( 'NONE', *, *, #11175, .T. ) ;
#5509 = EDGE_LOOP ( 'NONE', ( #10848, #3995, #12970, #4610 ) ) ;
#5510 = FACE_OUTER_BOUND ( 'NONE', #7000, .T. ) ;
#5511 = CARTESIAN_POINT ( 'NONE',  ( -1.969687200836069740, -2.871348872261489493, 0.1474822870563181620 ) ) ;
#5512 =( LENGTH_UNIT ( ) NAMED_UNIT ( * ) SI_UNIT ( $, .METRE. ) );
#5513 = CARTESIAN_POINT ( 'NONE',  ( -1.185322952774772842, 0.3350001135380079043, -0.05695403133965425829 ) ) ;
#5514 = CARTESIAN_POINT ( 'NONE',  ( -0.1618514667033796040, -0.1023622047244094474, 0.2161887458866224854 ) ) ;
#5515 = FACE_OUTER_BOUND ( 'NONE', #3837, .T. ) ;
#5516 = DIRECTION ( 'NONE',  ( -0.9453712468369984689, -0.3259957141648626711, 0.000000000000000000 ) ) ;
#5517 = CARTESIAN_POINT ( 'NONE',  ( -2.006299088073100201, -2.563573505072143099, -0.1516713583102864971 ) ) ;
#5518 = VERTEX_POINT ( 'NONE', #12019 ) ;
#5519 = EDGE_CURVE ( 'NONE', #796, #5799, #13624, .T. ) ;
#5520 = VERTEX_POINT ( 'NONE', #7149 ) ;
#5521 = EDGE_LOOP ( 'NONE', ( #17, #7088 ) ) ;
#5522 = ORIENTED_EDGE ( 'NONE', *, *, #7705, .T. ) ;
#5523 = CARTESIAN_POINT ( 'NONE',  ( -1.387074828437381280, -0.01127692237434234704, -0.07874015748031495954 ) ) ;
#5524 = DIRECTION ( 'NONE',  ( 0.000000000000000000, -1.000000000000000000, 0.000000000000000000 ) ) ;
#5525 = CARTESIAN_POINT ( 'NONE',  ( 0.05114323250695503031, 0.05905511811023622659, 0.08858267716535433989 ) ) ;
#5526 = CARTESIAN_POINT ( 'NONE',  ( -0.4307978335858689278, -0.09448818897637796532, 0.4279391777402706265 ) ) ;
#5527 = CARTESIAN_POINT ( 'NONE',  ( 0.1574803149606299191, -0.09842519685039370636, -0.5909884645248143498 ) ) ;
#5528 = FACE_OUTER_BOUND ( 'NONE', #1253, .T. ) ;
#5529 = CARTESIAN_POINT ( 'NONE',  ( -1.938021061366714815, -2.767805340190703678, -0.1776219654715974205 ) ) ;
#5530 = EDGE_LOOP ( 'NONE', ( #444, #14446, #2630, #2192 ) ) ;
#5531 = CARTESIAN_POINT ( 'NONE',  ( 0.1618514667033794374, -0.09842519685039372024, 0.2122517380126066888 ) ) ;
#5532 = DIRECTION ( 'NONE',  ( 0.000000000000000000, 0.000000000000000000, -1.000000000000000000 ) ) ;
#5533 = FACE_OUTER_BOUND ( 'NONE', #1506, .T. ) ;
#5534 = EDGE_LOOP ( 'NONE', ( #15087, #1464, #1923, #12218, #15397, #12381 ) ) ;
#5535 = VERTEX_POINT ( 'NONE', #6110 ) ;
#5536 = ORIENTED_EDGE ( 'NONE', *, *, #224, .T. ) ;
#5537 = CARTESIAN_POINT ( 'NONE',  ( 0.000000000000000000, 2.393700787401575436, 0.000000000000000000 ) ) ;
#5538 = ADVANCED_FACE ( 'NONE', ( #14281 ), #12168, .T. ) ;
#5539 = CARTESIAN_POINT ( 'NONE',  ( -0.7455328141524873997, 1.043307086614173151, 0.3622425942647021779 ) ) ;
#5540 = DIRECTION ( 'NONE',  ( 0.4999999999999998890, 0.000000000000000000, 0.8660254037844385966 ) ) ;
#5541 = DIRECTION ( 'NONE',  ( -1.000000000000000000, 0.000000000000000000, 0.000000000000000000 ) ) ;
#5542 = DIRECTION ( 'NONE',  ( -1.000000000000000000, -0.000000000000000000, -0.000000000000000000 ) ) ;
#5543 = CARTESIAN_POINT ( 'NONE',  ( 0.4749369078591172411, -0.4881889763779528324, 0.3514880584999470203 ) ) ;
#5544 = ORIENTED_EDGE ( 'NONE', *, *, #11278, .T. ) ;
#5545 = CARTESIAN_POINT ( 'NONE',  ( 1.141732283464566677, 4.044111181948214319E-16, -0.02559055118110236185 ) ) ;
#5546 = DIRECTION ( 'NONE',  ( 0.000000000000000000, 1.000000000000000000, 0.000000000000000000 ) ) ;
#5547 = DIRECTION ( 'NONE',  ( -0.000000000000000000, -1.000000000000000000, -0.000000000000000000 ) ) ;
#5548 = VERTEX_POINT ( 'NONE', #4788 ) ;
#5549 = EDGE_CURVE ( 'NONE', #6200, #4854, #13598, .T. ) ;
#5550 = CARTESIAN_POINT ( 'NONE',  ( -2.010991777528384983, -2.758467574604075434, 0.1561691687464104861 ) ) ;
#5551 = EDGE_CURVE ( 'NONE', #1254, #4333, #10870, .T. ) ;
#5552 = ORIENTED_EDGE ( 'NONE', *, *, #7286, .F. ) ;
#5553 = B_SPLINE_CURVE_WITH_KNOTS ( 'NONE', 3,
 ( #11457, #12718, #1977, #651, #4475, #15215 ),
 .UNSPECIFIED., .F., .F.,
 ( 4, 2, 4 ),
 ( -1.812136377038870460E-05, 0.0003725347987152521890, 0.0007631909612008931469 ),
 .UNSPECIFIED. ) ;
#5554 = ORIENTED_EDGE ( 'NONE', *, *, #8253, .T. ) ;
#5555 = ORIENTED_EDGE ( 'NONE', *, *, #4192, .T. ) ;
#5556 = EDGE_CURVE ( 'NONE', #10031, #13232, #7256, .T. ) ;
#5557 = DIRECTION ( 'NONE',  ( 0.000000000000000000, 0.000000000000000000, 1.000000000000000000 ) ) ;
#5558 = CARTESIAN_POINT ( 'NONE',  ( -0.002500327830562646542, 0.1591396728618060807, 8.151557182427766114E-17 ) ) ;
#5559 = DIRECTION ( 'NONE',  ( -0.5000000000000001110, 0.000000000000000000, 0.8660254037844385966 ) ) ;
#5560 = DIRECTION ( 'NONE',  ( -0.8660254037844381525, 0.000000000000000000, -0.5000000000000006661 ) ) ;
#5561 = AXIS2_PLACEMENT_3D ( 'NONE', #2879, #1786, #5375 ) ;
#5562 = VECTOR ( 'NONE', #13826, 39.37007874015748854 ) ;
#5563 = CARTESIAN_POINT ( 'NONE',  ( -1.574484809660414042, 0.1100025355989073528, 0.06175692796217682051 ) ) ;
#5564 = EDGE_LOOP ( 'NONE', ( #14055, #7496, #1571, #7150 ) ) ;
#5565 = CARTESIAN_POINT ( 'NONE',  ( -0.3441669734936866343, 2.010494531933507467, -0.03937007874015747977 ) ) ;
#5566 = CIRCLE ( 'NONE', #15086, 0.007874015748031482076 ) ;
#5567 = DIRECTION ( 'NONE',  ( 0.000000000000000000, 1.000000000000000000, 0.000000000000000000 ) ) ;
#5568 = CIRCLE ( 'NONE', #14846, 0.03937007874015754222 ) ;
#5569 = CARTESIAN_POINT ( 'NONE',  ( -1.579560458409220658, 0.1027931408840447314, 0.07190451969771766150 ) ) ;
#5570 = CYLINDRICAL_SURFACE ( 'NONE', #6686, 0.5511811023622046335 ) ;
#5571 = EDGE_CURVE ( 'NONE', #11092, #6371, #11374, .T. ) ;
#5572 = EDGE_LOOP ( 'NONE', ( #8738, #3737, #15161, #7354 ) ) ;
#5573 = ADVANCED_FACE ( 'NONE', ( #4727 ), #3544, .F. ) ;
#5574 = ORIENTED_EDGE ( 'NONE', *, *, #8763, .T. ) ;
#5575 = DIRECTION ( 'NONE',  ( -0.5000000000000035527, -0.000000000000000000, 0.8660254037844365982 ) ) ;
#5577 = EDGE_LOOP ( 'NONE', ( #10457, #3311, #5914, #8965 ) ) ;
#5576 = AXIS2_PLACEMENT_3D ( 'NONE', #11797, #15402, #13990 ) ;
#5578 = AXIS2_PLACEMENT_3D ( 'NONE', #7389, #10997, #2612 ) ;
#5579 = ORIENTED_EDGE ( 'NONE', *, *, #5612, .F. ) ;
#5580 = EDGE_CURVE ( 'NONE', #692, #12461, #1875, .T. ) ;
#5581 = AXIS2_PLACEMENT_3D ( 'NONE', #3009, #1825, #15006 ) ;
#5582 = PLANE ( 'NONE',  #5576 ) ;
#5583 = CARTESIAN_POINT ( 'NONE',  ( -2.010991777528384983, -2.758467574604075434, 0.1561691687464104861 ) ) ;
#5584 = SHAPE_REPRESENTATION_RELATIONSHIP ( 'NONE' , 'NONE' ,  #7785, #2758 ) ;
#5585 = CARTESIAN_POINT ( 'NONE',  ( -0.2952755905511810219, -0.02638708502139244100, -0.05905511811023622659 ) ) ;
#5586 = CARTESIAN_POINT ( 'NONE',  ( 0.5860051159906326523, -0.003937007874015747977, 0.1591122789105293422 ) ) ;
#5587 = DIRECTION ( 'NONE',  ( 8.673617379884051249E-15, 1.000000000000000000, 0.000000000000000000 ) ) ;
#5588 = VECTOR ( 'NONE', #5378, 39.37007874015748143 ) ;
#5589 = CARTESIAN_POINT ( 'NONE',  ( 0.03886060139087953863, 0.06736074103232488064, 0.08219815605943972536 ) ) ;
#5590 =( GEOMETRIC_REPRESENTATION_CONTEXT ( 3 ) GLOBAL_UNCERTAINTY_ASSIGNED_CONTEXT ( ( #10030 ) ) GLOBAL_UNIT_ASSIGNED_CONTEXT ( ( #12326, #9765, #4966 ) ) REPRESENTATION_CONTEXT ( 'NONE', 'WORKASPACE' ) );
#5591 = DIRECTION ( 'NONE',  ( 0.000000000000000000, 0.000000000000000000, 1.000000000000000000 ) ) ;
#5592 = CARTESIAN_POINT ( 'NONE',  ( -2.046508481693990689, -2.384357855454588115, -0.1146367095086625459 ) ) ;
#5593 = TOROIDAL_SURFACE ( 'NONE', #9375, 0.1535433070866141780, 0.003937007874015747977 ) ;
#5594 = AXIS2_PLACEMENT_3D ( 'NONE', #3004, #13744, #1682 ) ;
#5595 = ORIENTED_EDGE ( 'NONE', *, *, #8189, .F. ) ;
#5596 = PRODUCT_DEFINITION_FORMATION_WITH_SPECIFIED_SOURCE ( 'ANY', '', #8693, .NOT_KNOWN. ) ;
#5597 = ORIENTED_EDGE ( 'NONE', *, *, #720, .T. ) ;
#5598 = EDGE_LOOP ( 'NONE', ( #2773, #1878, #6162, #7159 ) ) ;
#5599 = ORIENTED_EDGE ( 'NONE', *, *, #8374, .F. ) ;
#5600 = EDGE_CURVE ( 'NONE', #2265, #2506, #14898, .T. ) ;
#5601 = AXIS2_PLACEMENT_3D ( 'NONE', #5223, #9952, #8834 ) ;
#5602 = AXIS2_PLACEMENT_3D ( 'NONE', #14378, #3958, #52 ) ;
#5603 = VECTOR ( 'NONE', #2511, 39.37007874015748143 ) ;
#5604 = CIRCLE ( 'NONE', #15125, 0.5984251968503937480 ) ;
#5605 = FACE_OUTER_BOUND ( 'NONE', #11699, .T. ) ;
#5606 = CARTESIAN_POINT ( 'NONE',  ( -0.1771653543307086243, -0.02638708502139245488, -0.03937007874015747977 ) ) ;
#5607 = DIRECTION ( 'NONE',  ( 0.5000000000000002220, 0.000000000000000000, 0.8660254037844384856 ) ) ;
#5608 = CIRCLE ( 'NONE', #4119, 0.08858267716535432601 ) ;
#5609 = EDGE_CURVE ( 'NONE', #15326, #12818, #1642, .T. ) ;
#5610 = CARTESIAN_POINT ( 'NONE',  ( -0.04489243112415021442, 0.1480120765563121277, 0.05194558739574919176 ) ) ;
#5611 = DIRECTION ( 'NONE',  ( -0.000000000000000000, 1.000000000000000000, -0.000000000000000000 ) ) ;
#5612 = EDGE_CURVE ( 'NONE', #10603, #2265, #4381, .T. ) ;
#5613 = CARTESIAN_POINT ( 'NONE',  ( -0.05905511811023622659, 1.338582677165354395, -0.5955041639236611228 ) ) ;
#5614 = CARTESIAN_POINT ( 'NONE',  ( 7.183951695785653893E-17, 2.440944881889763884, 0.5826771653543306728 ) ) ;
#5615 = CARTESIAN_POINT ( 'NONE',  ( -1.916733123353825841, -2.896650666303147492, -0.1268322157999333955 ) ) ;
#5616 = EDGE_LOOP ( 'NONE', ( #10648, #5499, #7529, #1074 ) ) ;
#5617 = LINE ( 'NONE', #7978, #12440 ) ;
#5618 = DIRECTION ( 'NONE',  ( 0.000000000000000000, -1.000000000000000000, 0.000000000000000000 ) ) ;
#5619 = AXIS2_PLACEMENT_3D ( 'NONE', #8183, #11862, #980 ) ;
#5620 = CIRCLE ( 'NONE', #8639, 0.5511811023622046335 ) ;
#5621 = ORIENTED_EDGE ( 'NONE', *, *, #5688, .T. ) ;
#5622 = ORIENTED_EDGE ( 'NONE', *, *, #14572, .T. ) ;
#5623 = LINE ( 'NONE', #6725, #11630 ) ;
#5624 = VECTOR ( 'NONE', #14983, 39.37007874015748143 ) ;
#5625 = AXIS2_PLACEMENT_3D ( 'NONE', #1667, #6424, #12397 ) ;
#5626 = CIRCLE ( 'NONE', #2890, 0.03937007874015754222 ) ;
#5627 = CARTESIAN_POINT ( 'NONE',  ( -1.276200637803905691, -0.1988000726501942539, -0.05905511811023622659 ) ) ;
#5628 = CARTESIAN_POINT ( 'NONE',  ( -1.967323444231620533, -2.828292283972135390, 0.1684768507627448786 ) ) ;
#5629 = CARTESIAN_POINT ( 'NONE',  ( -0.2325106836983179270, -0.1023622047244094474, 0.06483101467138334406 ) ) ;
#5630 = VECTOR ( 'NONE', #15320, 39.37007874015748143 ) ;
#5631 = LINE ( 'NONE', #786, #5875 ) ;
#5632 = ORIENTED_EDGE ( 'NONE', *, *, #378, .F. ) ;
#5633 = CARTESIAN_POINT ( 'NONE',  ( 0.06692913385832212347, -0.09842519685039370636, -0.5909884645248143498 ) ) ;
#5634 = DIRECTION ( 'NONE',  ( 0.000000000000000000, -1.000000000000000000, -0.000000000000000000 ) ) ;
#5635 = DIRECTION ( 'NONE',  ( 0.000000000000000000, 0.000000000000000000, 1.000000000000000000 ) ) ;
#5636 = CARTESIAN_POINT ( 'NONE',  ( -0.2393297813659119588, -0.4881889763779528324, 0.06089400679736758221 ) ) ;
#5637 = ORIENTED_EDGE ( 'NONE', *, *, #3521, .F. ) ;
#5638 = DIRECTION ( 'NONE',  ( -0.000000000000000000, -0.000000000000000000, -1.000000000000000000 ) ) ;
#5639 = CIRCLE ( 'NONE', #7899, 0.5984251968503937480 ) ;
#5640 = AXIS2_PLACEMENT_3D ( 'NONE', #234, #1626, #8818 ) ;
#5641 = TOROIDAL_SURFACE ( 'NONE', #14420, 2.814960629921260171, 0.01968503937007873988 ) ;
#5642 = ORIENTED_EDGE ( 'NONE', *, *, #14749, .F. ) ;
#5643 = ORIENTED_EDGE ( 'NONE', *, *, #7042, .T. ) ;
#5644 = AXIS2_PLACEMENT_3D ( 'NONE', #12328, #8889, #9118 ) ;
#5645 = PRODUCT_DEFINITION_SHAPE ( 'NONE', 'NONE',  #15481 ) ;
#5646 = FACE_OUTER_BOUND ( 'NONE', #14112, .T. ) ;
#5647 = LINE ( 'NONE', #12789, #12403 ) ;
#5648 = EDGE_CURVE ( 'NONE', #10031, #4530, #14652, .T. ) ;
#5649 = DIRECTION ( 'NONE',  ( 0.000000000000000000, -1.000000000000000000, 0.000000000000000000 ) ) ;
#5650 = CARTESIAN_POINT ( 'NONE',  ( 0.1259842519685039353, 2.440944881889763884, -0.04724409448818898266 ) ) ;
#5651 = DIRECTION ( 'NONE',  ( -0.4999999999999996114, 0.000000000000000000, -0.8660254037844389297 ) ) ;
#5652 = AXIS2_PLACEMENT_3D ( 'NONE', #3261, #8032, #10473 ) ;
#5653 = EDGE_CURVE ( 'NONE', #7766, #15055, #11360, .T. ) ;
#5654 = DIRECTION ( 'NONE',  ( 0.000000000000000000, 1.000000000000000000, 0.000000000000000000 ) ) ;
#5655 = ORIENTED_EDGE ( 'NONE', *, *, #3555, .F. ) ;
#5656 = DIRECTION ( 'NONE',  ( 1.000000000000000000, 0.000000000000000000, 0.000000000000000000 ) ) ;
#5657 = CIRCLE ( 'NONE', #15180, 0.003937007874015758385 ) ;
#5658 = CARTESIAN_POINT ( 'NONE',  ( -2.755905511811024056, 0.2985367441494412022, 0.1033464566929133965 ) ) ;
#5659 = ADVANCED_FACE ( 'NONE', ( #2989, #5237 ), #3931, .F. ) ;
#5660 = EDGE_LOOP ( 'NONE', ( #4439, #4972, #7779, #6215 ) ) ;
#5661 = ORIENTED_EDGE ( 'NONE', *, *, #13819, .F. ) ;
#5662 = DIRECTION ( 'NONE',  ( -1.000000000000000000, -0.000000000000000000, -3.476578583725179813E-16 ) ) ;
#5663 = EDGE_LOOP ( 'NONE', ( #3680, #13835, #322 ) ) ;
#5664 = AXIS2_PLACEMENT_3D ( 'NONE', #11134, #12631, #10207 ) ;
#5665 = ORIENTED_EDGE ( 'NONE', *, *, #5024, .F. ) ;
#5666 = VERTEX_POINT ( 'NONE', #4072 ) ;
#5667 = EDGE_CURVE ( 'NONE', #10393, #14556, #1884, .T. ) ;
#5668 = CARTESIAN_POINT ( 'NONE',  ( -0.1181102362204724532, 2.637795275590551825, 0.03937007874015747977 ) ) ;
#5669 = CARTESIAN_POINT ( 'NONE',  ( -1.983826685957652103, -2.834175259062820640, 0.1479833052181933617 ) ) ;
#5670 = EDGE_CURVE ( 'NONE', #2668, #13620, #14753, .T. ) ;
#5671 = DIRECTION ( 'NONE',  ( 0.6461174802832408970, -0.7632379718491709708, 0.000000000000000000 ) ) ;
#5672 = CARTESIAN_POINT ( 'NONE',  ( -0.4121618538092055584, -0.2952755905511811330, 0.1243101294532693024 ) ) ;
#5673 = CARTESIAN_POINT ( 'NONE',  ( -0.4783464566929145900, -0.4881889763779528324, 0.3534565624369550574 ) ) ;
#5674 = AXIS2_PLACEMENT_3D ( 'NONE', #12782, #10344, #15287 ) ;
#5675 = EDGE_CURVE ( 'NONE', #12501, #897, #10115, .T. ) ;
#5676 = CARTESIAN_POINT ( 'NONE',  ( 0.000000000000000000, 1.661417322834646049, 0.000000000000000000 ) ) ;
#5677 = DIRECTION ( 'NONE',  ( -1.000000000000000000, 0.000000000000000000, 0.000000000000000000 ) ) ;
#5678 = EDGE_LOOP ( 'NONE', ( #6503, #8981, #6160, #8472, #10741, #779 ) ) ;
#5679 = ORIENTED_EDGE ( 'NONE', *, *, #6760, .F. ) ;
#5680 = AXIS2_PLACEMENT_3D ( 'NONE', #1735, #5541, #784 ) ;
#5681 = ORIENTED_EDGE ( 'NONE', *, *, #636, .F. ) ;
#5682 = ORIENTED_EDGE ( 'NONE', *, *, #3505, .T. ) ;
#5683 = TOROIDAL_SURFACE ( 'NONE', #3884, 0.007874015748031495954, 0.003937007874015747977 ) ;
#5684 = CIRCLE ( 'NONE', #15460, 0.007874015748031516770 ) ;
#5685 = CARTESIAN_POINT ( 'NONE',  ( -1.572630165645363398, 0.1123721976955502078, -0.05999513677271276629 ) ) ;
#5686 = CARTESIAN_POINT ( 'NONE',  ( -0.06299212598414161146, -0.09842519685039372024, -0.5870514566507987197 ) ) ;
#5687 = AXIS2_PLACEMENT_3D ( 'NONE', #14398, #8439, #13449 ) ;
#5688 = EDGE_CURVE ( 'NONE', #12371, #6809, #12149, .T. ) ;
#5689 = FACE_OUTER_BOUND ( 'NONE', #3826, .T. ) ;
#5690 = FACE_OUTER_BOUND ( 'NONE', #8291, .T. ) ;
#5691 = DIRECTION ( 'NONE',  ( 0.000000000000000000, 0.000000000000000000, -1.000000000000000000 ) ) ;
#5692 = DIRECTION ( 'NONE',  ( 0.000000000000000000, 0.000000000000000000, 1.000000000000000000 ) ) ;
#5693 = CARTESIAN_POINT ( 'NONE',  ( -1.938116314515752947, -2.767513626600481835, -0.1578457079742228708 ) ) ;
#5694 = ORIENTED_EDGE ( 'NONE', *, *, #14342, .T. ) ;
#5695 = DIRECTION ( 'NONE',  ( 0.8483823383050430600, 0.5293839892290546079, -3.673339335687577446E-15 ) ) ;
#5696 = EDGE_CURVE ( 'NONE', #6393, #10309, #10644, .T. ) ;
#5697 = DIRECTION ( 'NONE',  ( 0.000000000000000000, 0.000000000000000000, -1.000000000000000000 ) ) ;
#5698 = AXIS2_PLACEMENT_3D ( 'NONE', #10904, #4950, #13952 ) ;
#5699 = ORIENTED_EDGE ( 'NONE', *, *, #6598, .F. ) ;
#5700 = VERTEX_POINT ( 'NONE', #12248 ) ;
#5701 =( GEOMETRIC_REPRESENTATION_CONTEXT ( 3 ) GLOBAL_UNCERTAINTY_ASSIGNED_CONTEXT ( ( #9080 ) ) GLOBAL_UNIT_ASSIGNED_CONTEXT ( ( #10155, #10298, #2777 ) ) REPRESENTATION_CONTEXT ( 'NONE', 'WORKASPACE' ) );
#5702 = ADVANCED_FACE ( 'NONE', ( #1505 ), #2675, .T. ) ;
#5703 = ORIENTED_EDGE ( 'NONE', *, *, #10059, .F. ) ;
#5704 = DIRECTION ( 'NONE',  ( -0.8660254037844384856, 6.349528607487585212E-15, 0.5000000000000004441 ) ) ;
#5705 = CARTESIAN_POINT ( 'NONE',  ( 0.2325106836984822400, -0.09842519685039370636, 0.06483101467147835140 ) ) ;
#5706 = CARTESIAN_POINT ( 'NONE',  ( -1.985311755390524624, -2.772329397582317778, 0.1771653543307079026 ) ) ;
#5707 = CARTESIAN_POINT ( 'NONE',  ( -0.1638199706403874467, -0.1023622047244094474, 0.2127791970528254695 ) ) ;
#5708 = SPHERICAL_SURFACE ( 'NONE', #3387, 0.003937007874015747977 ) ;
#5709 = VERTEX_POINT ( 'NONE', #11212 ) ;
#5710 = CARTESIAN_POINT ( 'NONE',  ( 0.5412721729274246885, 1.041728495490239714, 0.2430720373988119742 ) ) ;
#5711 = LINE ( 'NONE', #4710, #8356 ) ;
#5712 = DIRECTION ( 'NONE',  ( -0.8660254037844384856, 0.000000000000000000, -0.5000000000000002220 ) ) ;
#5713 = ORIENTED_EDGE ( 'NONE', *, *, #1778, .F. ) ;
#5714 = CARTESIAN_POINT ( 'NONE',  ( 0.1540707661268329032, -0.09448818897637796532, -0.5890199605878065903 ) ) ;
#5715 = ORIENTED_EDGE ( 'NONE', *, *, #7024, .T. ) ;
#5716 = ADVANCED_FACE ( 'NONE', ( #494 ), #7637, .F. ) ;
#5717 = EDGE_LOOP ( 'NONE', ( #15178, #1264, #4277 ) ) ;
#5718 = VERTEX_POINT ( 'NONE', #11451 ) ;
#5719 = DIRECTION ( 'NONE',  ( 0.8660254037844347108, -0.000000000000000000, -0.5000000000000069944 ) ) ;
#5720 = CARTESIAN_POINT ( 'NONE',  ( -1.253866366384063902, 0.1355266887446167634, 0.03937007874015747977 ) ) ;
#5721 = CARTESIAN_POINT ( 'NONE',  ( -0.3137366569588388998, -0.2952755905511811330, 0.2947875711430708590 ) ) ;
#5722 = CARTESIAN_POINT ( 'NONE',  ( 0.1181102362204724671, 2.444206406002937815, -0.03937007874015747977 ) ) ;
#5723 = DIRECTION ( 'NONE',  ( 0.000000000000000000, -1.000000000000000000, 0.000000000000000000 ) ) ;
#5724 = FACE_OUTER_BOUND ( 'NONE', #5660, .T. ) ;
#5725 = EDGE_LOOP ( 'NONE', ( #5899, #13158, #5247, #13901 ) ) ;
#5726 = CARTESIAN_POINT ( 'NONE',  ( -1.958689581535855373, -2.899312375919938400, -0.1241928182215008836 ) ) ;
#5727 = DIRECTION ( 'NONE',  ( 0.4999999999999922284, -0.000000000000000000, -0.8660254037844430375 ) ) ;
#5728 = CARTESIAN_POINT ( 'NONE',  ( 0.4749369078591172411, -0.4881889763779528324, 0.3514880584999470203 ) ) ;
#5729 = DIRECTION ( 'NONE',  ( -8.673617379884032317E-15, 0.000000000000000000, -1.000000000000000000 ) ) ;
#5730 = CARTESIAN_POINT ( 'NONE',  ( 6.846450609406462919E-17, 0.5590551181102362266, -0.5590551181102362266 ) ) ;
#5731 = SURFACE_SIDE_STYLE ('',( #12799 ) ) ;
#5732 = ORIENTED_EDGE ( 'NONE', *, *, #6051, .F. ) ;
#5733 = ORIENTED_EDGE ( 'NONE', *, *, #2020, .T. ) ;
#5734 = CARTESIAN_POINT ( 'NONE',  ( 0.05905511811023622659, 1.338582677165354395, -0.5955041639236611228 ) ) ;
#5735 = VERTEX_POINT ( 'NONE', #724 ) ;
#5736 = ORIENTED_EDGE ( 'NONE', *, *, #6481, .F. ) ;
#5737 = ORIENTED_EDGE ( 'NONE', *, *, #5167, .T. ) ;
#5738 = FACE_OUTER_BOUND ( 'NONE', #6452, .T. ) ;
#5739 = ADVANCED_FACE ( 'NONE', ( #3224 ), #5708, .T. ) ;
#5740 = DIRECTION ( 'NONE',  ( 0.000000000000000000, -1.000000000000000000, 0.000000000000000000 ) ) ;
#5741 = CARTESIAN_POINT ( 'NONE',  ( -1.906721773844014534, -2.925049931903382916, 0.09056425822888818089 ) ) ;
#5742 = SHAPE_REPRESENTATION_RELATIONSHIP ( 'NONE' , 'NONE' ,  #12105, #14739 ) ;
#5743 = DIRECTION ( 'NONE',  ( 0.000000000000000000, 0.000000000000000000, -1.000000000000000000 ) ) ;
#5744 = DIRECTION ( 'NONE',  ( 0.4999999999999919509, -0.000000000000000000, -0.8660254037844432595 ) ) ;
#5745 = DIRECTION ( 'NONE',  ( 3.476578583725179813E-16, 0.000000000000000000, -1.000000000000000000 ) ) ;
#5746 = DIRECTION ( 'NONE',  ( 0.8660254037844309360, 0.000000000000000000, -0.5000000000000134337 ) ) ;
#5747 = DIRECTION ( 'NONE',  ( -0.000000000000000000, -1.000000000000000000, -0.000000000000000000 ) ) ;
#5748 = CARTESIAN_POINT ( 'NONE',  ( -0.2362204724409448231, -0.02638708502139245488, -0.05905511811023622659 ) ) ;
#5749 = CARTESIAN_POINT ( 'NONE',  ( 0.7052242655755273093, -1.858423098537180129, 0.1033464566929129108 ) ) ;
#5750 = EDGE_LOOP ( 'NONE', ( #2924, #10695, #11223, #10950, #5412, #15433, #7510 ) ) ;
#5751 = ORIENTED_EDGE ( 'NONE', *, *, #8214, .F. ) ;
#5752 = EDGE_CURVE ( 'NONE', #7829, #4717, #5479, .T. ) ;
#5753 = VERTEX_POINT ( 'NONE', #4389 ) ;
#5754 = EDGE_CURVE ( 'NONE', #11599, #9415, #5631, .T. ) ;
#5755 = ORIENTED_EDGE ( 'NONE', *, *, #4043, .T. ) ;
#5756 = EDGE_CURVE ( 'NONE', #7384, #15055, #4876, .T. ) ;
#5757 = DIRECTION ( 'NONE',  ( 0.5000000000000035527, 0.000000000000000000, -0.8660254037844365982 ) ) ;
#5758 = CARTESIAN_POINT ( 'NONE',  ( -0.04047196874988589349, 0.1700209211169187440, 0.02286660095798146927 ) ) ;
#5759 = CARTESIAN_POINT ( 'NONE',  ( -0.03747986570939450257, -0.1642921853714506275, -0.04794034192644638925 ) ) ;
#5760 = CYLINDRICAL_SURFACE ( 'NONE', #3072, 0.003937007874015754916 ) ;
#5761 = CARTESIAN_POINT ( 'NONE',  ( 0.5452755905511544876, -0.4921259842519685179, 0.2375319020879054499 ) ) ;
#5762 = ORIENTED_EDGE ( 'NONE', *, *, #1943, .F. ) ;
#5763 = CYLINDRICAL_SURFACE ( 'NONE', #2442, 0.003937007874015724558 ) ;
#5764 = CARTESIAN_POINT ( 'NONE',  ( -0.05175539059627463218, 0.000000000000000000, 0.07475334604056275978 ) ) ;
#5765 = CARTESIAN_POINT ( 'NONE',  ( 9.360245101547351149E-18, 0.07093549527207514138, 0.07900545476875124595 ) ) ;
#5766 = PRODUCT_DEFINITION_SHAPE ( 'NONE', 'NONE',  #561 ) ;
#5767 = EDGE_LOOP ( 'NONE', ( #3262, #2065, #2791 ) ) ;
#5768 =( BOUNDED_CURVE ( )  B_SPLINE_CURVE ( 3, ( #8180, #12645, #1916, #5563 ),
 .UNSPECIFIED., .F., .T. ) 
 B_SPLINE_CURVE_WITH_KNOTS ( ( 4, 4 ),
 ( 1.570796326794899667, 2.100913045340505825 ),
 .UNSPECIFIED. ) 
 CURVE ( )  GEOMETRIC_REPRESENTATION_ITEM ( )  RATIONAL_B_SPLINE_CURVE ( ( 1.000000000000000000, 0.9767181429356339706, 0.9767181429356339706, 1.000000000000000000 ) ) 
 REPRESENTATION_ITEM ( '' )  );
#5769 = ORIENTED_EDGE ( 'NONE', *, *, #7214, .F. ) ;
#5770 = EDGE_CURVE ( 'NONE', #8667, #4753, #2870, .T. ) ;
#5771 = ORIENTED_EDGE ( 'NONE', *, *, #5359, .F. ) ;
#5772 = DIRECTION ( 'NONE',  ( 1.000000000000000000, 0.000000000000000000, 0.000000000000000000 ) ) ;
#5773 = EDGE_CURVE ( 'NONE', #13377, #13441, #1972, .T. ) ;
#5774 = CARTESIAN_POINT ( 'NONE',  ( 0.5610236220472175628, -0.09842519685039370636, 0.2102555114175294892 ) ) ;
#5775 = CARTESIAN_POINT ( 'NONE',  ( -1.928549775957746570, -2.939860280416023652, -0.05881069861817015548 ) ) ;
#5776 = CARTESIAN_POINT ( 'NONE',  ( 0.05314960629921190033, -0.09842519685039370636, 0.09205781851251784720 ) ) ;
#5777 = FACE_OUTER_BOUND ( 'NONE', #3233, .T. ) ;
#5778 = CARTESIAN_POINT ( 'NONE',  ( -1.181096721701077046, 0.3434326084059158846, -0.04453596627218543019 ) ) ;
#5779 = ORIENTED_EDGE ( 'NONE', *, *, #2782, .T. ) ;
#5780 = DIRECTION ( 'NONE',  ( -1.000000000000000000, -4.625929269271485914E-16, -2.309263891220325920E-14 ) ) ;
#5781 = ADVANCED_FACE ( 'NONE', ( #4297 ), #9176, .T. ) ;
#5782 = DIRECTION ( 'NONE',  ( 0.000000000000000000, -1.000000000000000000, 0.000000000000000000 ) ) ;
#5783 = FACE_OUTER_BOUND ( 'NONE', #5953, .T. ) ;
#5784 = CARTESIAN_POINT ( 'NONE',  ( 0.2359202325322792559, -0.4921259842519685179, 0.06286251073447048088 ) ) ;
#5785 = VERTEX_POINT ( 'NONE', #6893 ) ;
#5786 = DIRECTION ( 'NONE',  ( -0.000000000000000000, -1.000000000000000000, -0.000000000000000000 ) ) ;
#5787 = ORIENTED_EDGE ( 'NONE', *, *, #7503, .F. ) ;
#5788 = ORIENTED_EDGE ( 'NONE', *, *, #11515, .F. ) ;
#5789 = EDGE_LOOP ( 'NONE', ( #10728, #8349 ) ) ;
#5790 = EDGE_CURVE ( 'NONE', #11240, #4737, #9899, .T. ) ;
#5791 = FACE_OUTER_BOUND ( 'NONE', #8136, .T. ) ;
#5792 = DIRECTION ( 'NONE',  ( -0.000000000000000000, -1.000000000000000000, -0.000000000000000000 ) ) ;
#5793 = CARTESIAN_POINT ( 'NONE',  ( 0.5629921259843070347, -0.4881889763779528324, 0.2068459625837795746 ) ) ;
#5794 = DIRECTION ( 'NONE',  ( 0.000000000000000000, 1.000000000000000000, 0.000000000000000000 ) ) ;
#5795 = ITEM_DEFINED_TRANSFORMATION ( 'NONE', 'NONE', #3865,  #11481 ) ;
#5796 = CARTESIAN_POINT ( 'NONE',  ( -2.755905511811024056, -2.772329397582842248, 0.1771653543307079026 ) ) ;
#5797 = CARTESIAN_POINT ( 'NONE',  ( 0.000000000000000000, 2.433070866141732846, -0.5905511811023621549 ) ) ;
#5798 = ADVANCED_FACE ( 'NONE', ( #12844 ), #7376, .F. ) ;
#5799 = VERTEX_POINT ( 'NONE', #2032 ) ;
#5800 = CARTESIAN_POINT ( 'NONE',  ( -0.07874015748031494566, 0.1442356988431297837, 0.03937007874015747977 ) ) ;
#5801 = EDGE_CURVE ( 'NONE', #7004, #9440, #2128, .T. ) ;
#5802 = CARTESIAN_POINT ( 'NONE',  ( 0.2681506793018587631, -0.1023622047244094474, 0.03207310886168001501 ) ) ;
#5803 = DIRECTION ( 'NONE',  ( 1.000000000000000000, -0.000000000000000000, 1.224646799147353207E-16 ) ) ;
#5804 = EDGE_LOOP ( 'NONE', ( #7052, #12741, #10671, #11361 ) ) ;
#5805 = DIRECTION ( 'NONE',  ( 1.060575238724906792E-16, 1.000000000000000000, 6.123233995736767268E-17 ) ) ;
#5806 = ORIENTED_EDGE ( 'NONE', *, *, #4098, .F. ) ;
#5807 = ORIENTED_EDGE ( 'NONE', *, *, #7777, .T. ) ;
#5808 = VERTEX_POINT ( 'NONE', #11591 ) ;
#5809 = LINE ( 'NONE', #6623, #11122 ) ;
#5810 = AXIS2_PLACEMENT_3D ( 'NONE', #2317, #14314, #7190 ) ;
#5811 = AXIS2_PLACEMENT_3D ( 'NONE', #13919, #7728, #1708 ) ;
#5812 = DIRECTION ( 'NONE',  ( -0.8660254037844398178, 0.000000000000000000, 0.4999999999999979461 ) ) ;
#5813 = CARTESIAN_POINT ( 'NONE',  ( -1.957251767100264495, -2.772329397581817734, -0.1771653543307079026 ) ) ;
#5814 = CIRCLE ( 'NONE', #5320, 0.003937007874015758385 ) ;
#5815 = FACE_OUTER_BOUND ( 'NONE', #8005, .T. ) ;
#5816 = CARTESIAN_POINT ( 'NONE',  ( 0.3294846884549027521, -0.2952755905511811330, 0.2675111804726952314 ) ) ;
#5817 = FACE_OUTER_BOUND ( 'NONE', #13946, .T. ) ;
#5818 = CARTESIAN_POINT ( 'NONE',  ( -2.090051324975637836, -1.782906609499567585, -0.08465180024024840377 ) ) ;
#5819 = DIRECTION ( 'NONE',  ( 0.000000000000000000, 0.000000000000000000, -1.000000000000000000 ) ) ;
#5820 = AXIS2_PLACEMENT_3D ( 'NONE', #9066, #12451, #10976 ) ;
#5821 = AXIS2_PLACEMENT_3D ( 'NONE', #14783, #11408, #7878 ) ;
#5822 = EDGE_LOOP ( 'NONE', ( #489, #4309, #8392, #11620 ) ) ;
#5823 = VECTOR ( 'NONE', #10391, 39.37007874015748854 ) ;
#5824 = EDGE_LOOP ( 'NONE', ( #7610, #9562, #12301, #6949 ) ) ;
#5825 = AXIS2_PLACEMENT_3D ( 'NONE', #4300, #13957, #1741 ) ;
#5826 = ORIENTED_EDGE ( 'NONE', *, *, #12561, .T. ) ;
#5827 = ORIENTED_EDGE ( 'NONE', *, *, #59, .T. ) ;
#5828 = DIRECTION ( 'NONE',  ( -0.5801894994542512451, -0.8144815189573213488, 0.000000000000000000 ) ) ;
#5829 = CIRCLE ( 'NONE', #1845, 0.03937007874015751446 ) ;
#5830 = VECTOR ( 'NONE', #4963, 39.37007874015748143 ) ;
#5831 = DIRECTION ( 'NONE',  ( -1.000000000000000000, 1.224646799147296261E-16, 0.000000000000000000 ) ) ;
#5832 = EDGE_CURVE ( 'NONE', #1180, #12971, #8060, .T. ) ;
#5833 = AXIS2_PLACEMENT_3D ( 'NONE', #552, #6251, #8778 ) ;
#5834 = CARTESIAN_POINT ( 'NONE',  ( -0.5412478373021294420, 1.346456692913385877, 0.2362233606508100381 ) ) ;
#5835 = VECTOR ( 'NONE', #3518, 39.37007874015748143 ) ;
#5836 = CARTESIAN_POINT ( 'NONE',  ( 0.06692913385832209572, -0.2952755905511811330, -0.4584677793364516640 ) ) ;
#5837 = DIRECTION ( 'NONE',  ( 0.000000000000000000, 1.000000000000000000, 0.000000000000000000 ) ) ;
#5838 = ADVANCED_FACE ( 'NONE', ( #10500 ), #4267, .F. ) ;
#5839 = VERTEX_POINT ( 'NONE', #4623 ) ;
#5840 = DIRECTION ( 'NONE',  ( -0.000000000000000000, -1.000000000000000000, -0.000000000000000000 ) ) ;
#5841 = LINE ( 'NONE', #11992, #4142 ) ;
#5842 = ORIENTED_EDGE ( 'NONE', *, *, #3235, .T. ) ;
#5843 = EDGE_CURVE ( 'NONE', #925, #13968, #5933, .T. ) ;
#5844 = ORIENTED_EDGE ( 'NONE', *, *, #14885, .T. ) ;
#5845 = CIRCLE ( 'NONE', #5339, 0.01968503937007875723 ) ;
#5846 = CIRCLE ( 'NONE', #3114, 0.5433070866141731514 ) ;
#5847 = VECTOR ( 'NONE', #1801, 39.37007874015748143 ) ;
#5848 = AXIS2_PLACEMENT_3D ( 'NONE', #7961, #15250, #13996 ) ;
#5849 = ORIENTED_EDGE ( 'NONE', *, *, #9997, .T. ) ;
#5850 = AXIS2_PLACEMENT_3D ( 'NONE', #14830, #1912, #3070 ) ;
#5851 = FACE_OUTER_BOUND ( 'NONE', #8665, .T. ) ;
#5852 = DIRECTION ( 'NONE',  ( 0.000000000000000000, 0.000000000000000000, 1.000000000000000000 ) ) ;
#5853 = EDGE_CURVE ( 'NONE', #12623, #1730, #7885, .T. ) ;
#5854 = DIRECTION ( 'NONE',  ( -0.8660254037844431485, 4.956352788505159323E-16, -0.4999999999999918954 ) ) ;
#5855 = CARTESIAN_POINT ( 'NONE',  ( -1.925023804306413622, -2.949475017834376711, -0.01222676651384939014 ) ) ;
#5856 = VECTOR ( 'NONE', #7621, 39.37007874015748143 ) ;
#5857 = DIRECTION ( 'NONE',  ( 1.000000000000000000, 1.734723475976817507E-14, 0.000000000000000000 ) ) ;
#5858 = AXIS2_PLACEMENT_3D ( 'NONE', #11788, #13980, #2056 ) ;
#5859 = B_SPLINE_CURVE_WITH_KNOTS ( 'NONE', 3,
 ( #6401, #11195, #3915, #3824 ),
 .UNSPECIFIED., .F., .F.,
 ( 4, 4 ),
 ( -2.828444569876537743E-06, 0.0002461255424396399509 ),
 .UNSPECIFIED. ) ;
#5860 = FACE_OUTER_BOUND ( 'NONE', #13525, .T. ) ;
#5861 = EDGE_CURVE ( 'NONE', #3171, #14774, #7045, .T. ) ;
#5862 = AXIS2_PLACEMENT_3D ( 'NONE', #14508, #8538, #13313 ) ;
#5863 = VERTEX_POINT ( 'NONE', #16 ) ;
#5864 = CARTESIAN_POINT ( 'NONE',  ( -2.003370110189420572, -2.780373828034933492, 0.1578437203291705448 ) ) ;
#5865 =( BOUNDED_SURFACE ( )  B_SPLINE_SURFACE ( 3, 2, ( 
 ( #8728, #1750, #12324 ),
 ( #11293, #3003, #9985 ),
 ( #7769, #14764, #1816 ),
 ( #6581, #7935, #14121 ),
 ( #13972, #6992, #3238 ),
 ( #661, #12641, #1987 ),
 ( #15296, #6747, #11704 ),
 ( #1911, #6815, #4406 ),
 ( #3160, #5420, #739 ),
 ( #11536, #8175, #13807 ) ),
 .UNSPECIFIED., .F., .F., .T. ) 
 B_SPLINE_SURFACE_WITH_KNOTS ( ( 4, 2, 2, 2, 4 ),
 ( 3, 3 ),
 ( 0.004868238565068919166, 0.005367227319713948480, 0.005866216074358976927, 0.006365204829004005374, 0.006864193583649034688 ),
 ( 0.000000000000000000, 1.000000000000000000 ),
 .UNSPECIFIED. ) 
 GEOMETRIC_REPRESENTATION_ITEM ( )  RATIONAL_B_SPLINE_SURFACE ( (
 ( 1.000000000000000000, 0.7071067811865475727, 1.000000000000000000),
 ( 1.000000000000000000, 0.7015640395779025873, 1.000000000000000000),
 ( 1.000000000000000000, 0.6956970733052282307, 1.000000000000000000),
 ( 1.000000000000000000, 0.6834122233792360168, 1.000000000000000000),
 ( 1.000000000000000000, 0.6772899333991397874, 1.000000000000000000),
 ( 1.000000000000000000, 0.6655724472122266366, 1.000000000000000000),
 ( 1.000000000000000000, 0.6602173990144631910, 1.000000000000000000),
 ( 1.000000000000000000, 0.6512508157287247856, 1.000000000000000000),
 ( 1.000000000000000000, 0.6477776718209199425, 1.000000000000000000),
 ( 1.000000000000000000, 0.6456929433798523910, 1.000000000000000000) ) ) 
 REPRESENTATION_ITEM ( '' )  SURFACE ( )  );
#5866 = CYLINDRICAL_SURFACE ( 'NONE', #1361, 0.003937007874015758385 ) ;
#5867 = CIRCLE ( 'NONE', #14647, 0.007874015748031516770 ) ;
#5868 = CARTESIAN_POINT ( 'NONE',  ( -0.2393297813659120143, -0.4881889763779528324, 0.06089400679736763772 ) ) ;
#5869 = DIRECTION ( 'NONE',  ( 0.000000000000000000, 0.000000000000000000, -1.000000000000000000 ) ) ;
#5870 = ORIENTED_EDGE ( 'NONE', *, *, #12365, .F. ) ;
#5871 = ADVANCED_FACE ( 'NONE', ( #5860 ), #564, .T. ) ;
#5872 = EDGE_CURVE ( 'NONE', #6983, #7883, #9658, .T. ) ;
#5873 = ORIENTED_EDGE ( 'NONE', *, *, #6481, .T. ) ;
#5874 = ORIENTED_EDGE ( 'NONE', *, *, #1698, .F. ) ;
#5876 = VERTEX_POINT ( 'NONE', #3046 ) ;
#5875 = VECTOR ( 'NONE', #10333, 39.37007874015748143 ) ;
#5877 = CIRCLE ( 'NONE', #3405, 0.7007874015748031260 ) ;
#5878 = ORIENTED_EDGE ( 'NONE', *, *, #14416, .T. ) ;
#5879 = DIRECTION ( 'NONE',  ( 0.5000000000000134337, 0.000000000000000000, 0.8660254037844309360 ) ) ;
#5880 = DIRECTION ( 'NONE',  ( -1.000000000000000000, 0.000000000000000000, 0.000000000000000000 ) ) ;
#5881 = AXIS2_PLACEMENT_3D ( 'NONE', #5224, #7740, #5379 ) ;
#5882 = CARTESIAN_POINT ( 'NONE',  ( -1.419615703517932426, -0.01226548420975529831, 0.07609966981162474831 ) ) ;
#5883 = CYLINDRICAL_SURFACE ( 'NONE', #7599, 0.007874015748031499423 ) ;
#5884 = CONTEXT_DEPENDENT_SHAPE_REPRESENTATION ( #7500, #12786 ) ;
#5885 = CARTESIAN_POINT ( 'NONE',  ( 0.000000000000000000, 0.3464566929133857109, -0.5590551181102362266 ) ) ;
#5886 = ORIENTED_EDGE ( 'NONE', *, *, #10590, .F. ) ;
#5887 = LINE ( 'NONE', #12796, #10912 ) ;
#5888 = DIRECTION ( 'NONE',  ( -0.000000000000000000, -1.000000000000000000, 0.000000000000000000 ) ) ;
#5889 = CIRCLE ( 'NONE', #158, 0.5984251968503937480 ) ;
#5890 = CIRCLE ( 'NONE', #8653, 0.7086614173228346081 ) ;
#5891 = LINE ( 'NONE', #4730, #8457 ) ;
#5892 = VECTOR ( 'NONE', #3305, 39.37007874015748143 ) ;
#5893 = CARTESIAN_POINT ( 'NONE',  ( -0.2373612774289040883, -0.1023622047244094474, 0.06430355563116459117 ) ) ;
#5894 = ADVANCED_FACE ( 'NONE', ( #7813 ), #9305, .T. ) ;
#5895 = AXIS2_PLACEMENT_3D ( 'NONE', #7537, #7311, #10770 ) ;
#5896 = ORIENTED_EDGE ( 'NONE', *, *, #1675, .T. ) ;
#5897 = EDGE_LOOP ( 'NONE', ( #4355, #6093, #8243, #13175 ) ) ;
#5898 = VERTEX_POINT ( 'NONE', #10180 ) ;
#5899 = ORIENTED_EDGE ( 'NONE', *, *, #797, .F. ) ;
#5900 = ADVANCED_FACE ( 'NONE', ( #1952 ), #6634, .T. ) ;
#5901 = ORIENTED_EDGE ( 'NONE', *, *, #8788, .F. ) ;
#5902 = AXIS2_PLACEMENT_3D ( 'NONE', #8570, #6214, #14471 ) ;
#5903 = B_SPLINE_CURVE_WITH_KNOTS ( 'NONE', 3,
 ( #11422, #699, #5456, #10245 ),
 .UNSPECIFIED., .F., .F.,
 ( 4, 4 ),
 ( 2.006738551125145802E-07, 0.0009905856238791982925 ),
 .UNSPECIFIED. ) ;
#5904 = DIRECTION ( 'NONE',  ( -1.000000000000000000, 0.000000000000000000, 0.000000000000000000 ) ) ;
#5905 = CARTESIAN_POINT ( 'NONE',  ( -1.953792234680448159, -2.783667854742955416, 0.1771653543307004364 ) ) ;
#5906 = LENGTH_MEASURE_WITH_UNIT ( LENGTH_MEASURE( 0.02539999999999999897 ), #14147 );
#5907 = SURFACE_STYLE_USAGE ( .BOTH. , #9460 ) ;
#5908 = AXIS2_PLACEMENT_3D ( 'NONE', #4180, #5335, #744 ) ;
#5909 = DIRECTION ( 'NONE',  ( -0.4999999999999998335, 0.000000000000000000, -0.8660254037844388186 ) ) ;
#5910 = DIRECTION ( 'NONE',  ( 0.000000000000000000, 0.000000000000000000, 1.000000000000000000 ) ) ;
#5911 = DIRECTION ( 'NONE',  ( -0.8660254037844365982, 0.000000000000000000, -0.5000000000000035527 ) ) ;
#5912 = CARTESIAN_POINT ( 'NONE',  ( 0.000000000000000000, -0.4881889763779528324, -0.5870514566507987197 ) ) ;
#5913 =( NAMED_UNIT ( * ) SI_UNIT ( $, .STERADIAN. ) SOLID_ANGLE_UNIT ( ) );
#5914 = ORIENTED_EDGE ( 'NONE', *, *, #12751, .T. ) ;
#5915 = ORIENTED_EDGE ( 'NONE', *, *, #5957, .F. ) ;
#5916 = ORIENTED_EDGE ( 'NONE', *, *, #14623, .T. ) ;
#5917 = ORIENTED_EDGE ( 'NONE', *, *, #6598, .T. ) ;
#5918 = ADVANCED_FACE ( 'NONE', ( #5384 ), #5464, .T. ) ;
#5919 = CARTESIAN_POINT ( 'NONE',  ( -0.2952755905511810219, -0.02638708502139244794, 0.03937007874015747977 ) ) ;
#5920 = AXIS2_PLACEMENT_3D ( 'NONE', #10251, #1871, #706 ) ;
#5921 = TOROIDAL_SURFACE ( 'NONE', #206, 0.007874015748031495954, 0.003937007874015747977 ) ;
#5922 = DIRECTION ( 'NONE',  ( 0.000000000000000000, 0.000000000000000000, -1.000000000000000000 ) ) ;
#5923 = DIRECTION ( 'NONE',  ( 0.000000000000000000, 0.000000000000000000, 1.000000000000000000 ) ) ;
#5924 = CARTESIAN_POINT ( 'NONE',  ( 0.05114323250695503031, 0.000000000000000000, 0.08858267716535433989 ) ) ;
#5925 = AXIS2_PLACEMENT_3D ( 'NONE', #7904, #5695, #12690 ) ;
#5926 = DIRECTION ( 'NONE',  ( 0.5000000000000001110, 0.000000000000000000, 0.8660254037844385966 ) ) ;
#5927 = ORIENTED_EDGE ( 'NONE', *, *, #1012, .F. ) ;
#5928 = CYLINDRICAL_SURFACE ( 'NONE', #11188, 0.6692913385826770867 ) ;
#5929 = CARTESIAN_POINT ( 'NONE',  ( -0.000000000000000000, -0.09842519685039370636, -0.5870514566507987197 ) ) ;
#5930 = DIRECTION ( 'NONE',  ( -0.000000000000000000, -1.000000000000000000, 0.000000000000000000 ) ) ;
#5931 = AXIS2_PLACEMENT_3D ( 'NONE', #2987, #9019, #6650 ) ;
#5932 = ORIENTED_EDGE ( 'NONE', *, *, #7203, .T. ) ;
#5933 = B_SPLINE_CURVE_WITH_KNOTS ( 'NONE', 3,
 ( #7125, #9728, #2270, #10735, #14499, #85, #11832, #14333, #13075, #13240 ),
 .UNSPECIFIED., .F., .F.,
 ( 4, 2, 2, 2, 4 ),
 ( 0.000000000000000000, 0.003638111460239016465, 0.007276222920478032929, 0.01455244584095600514, 0.02910489168191195131 ),
 .UNSPECIFIED. ) ;
#5934 = VERTEX_POINT ( 'NONE', #12760 ) ;
#5935 = VECTOR ( 'NONE', #2407, 39.37007874015748143 ) ;
#5936 = ORIENTED_EDGE ( 'NONE', *, *, #7029, .T. ) ;
#5937 = AXIS2_PLACEMENT_3D ( 'NONE', #6426, #4237, #729 ) ;
#5938 = EDGE_CURVE ( 'NONE', #3128, #6292, #11908, .T. ) ;
#5939 = DIRECTION ( 'NONE',  ( -0.000000000000000000, -1.000000000000000000, -0.000000000000000000 ) ) ;
#5940 = DIRECTION ( 'NONE',  ( 0.000000000000000000, 0.000000000000000000, 1.000000000000000000 ) ) ;
#5941 = CARTESIAN_POINT ( 'NONE',  ( -1.933241136925626824, -2.926924945584949533, -0.08676524546727019949 ) ) ;
#5942 = EDGE_CURVE ( 'NONE', #9581, #5785, #7245, .T. ) ;
#5943 = CARTESIAN_POINT ( 'NONE',  ( -1.967325247738501703, -2.828286626395489556, -0.1684772211806224995 ) ) ;
#5944 = DIRECTION ( 'NONE',  ( 0.000000000000000000, 0.000000000000000000, -1.000000000000000000 ) ) ;
#5945 = LINE ( 'NONE', #3456, #12976 ) ;
#5946 = B_SPLINE_CURVE_WITH_KNOTS ( 'NONE', 3,
 ( #2037, #2121, #962, #3295, #8065, #6897, #3533, #1033, #15284, #10505 ),
 .UNSPECIFIED., .F., .F.,
 ( 4, 2, 2, 2, 4 ),
 ( 7.655474390655438337E-20, 0.0006605458767770998286, 0.001321091753554199440, 0.001981637630331298944, 0.002642183507108398881 ),
 .UNSPECIFIED. ) ;
#5947 = ORIENTED_EDGE ( 'NONE', *, *, #1310, .F. ) ;
#5948 = CARTESIAN_POINT ( 'NONE',  ( -1.946003491706560506, -2.930556585132634506, -0.04593750474734910327 ) ) ;
#5949 = CARTESIAN_POINT ( 'NONE',  ( -1.276200637803905691, -0.1988000726501942539, 0.1033464566929132716 ) ) ;
#5950 = VECTOR ( 'NONE', #8773, 39.37007874015748143 ) ;
#5951 = FACE_OUTER_BOUND ( 'NONE', #2869, .T. ) ;
#5952 = CARTESIAN_POINT ( 'NONE',  ( -0.06692913385826772255, 0.000000000000000000, -0.5946706712680680518 ) ) ;
#5953 = EDGE_LOOP ( 'NONE', ( #11506, #11786, #3818, #3384, #10512, #11482 ) ) ;
#5954 = EDGE_CURVE ( 'NONE', #6722, #1731, #12533, .T. ) ;
#5955 = ORIENTED_EDGE ( 'NONE', *, *, #3366, .F. ) ;
#5956 = CIRCLE ( 'NONE', #2472, 0.003937007874015758385 ) ;
#5957 = EDGE_CURVE ( 'NONE', #13359, #11417, #7137, .T. ) ;
#5958 = DIRECTION ( 'NONE',  ( 0.4999999999999966693, 0.000000000000000000, -0.8660254037844405950 ) ) ;
#5959 = CYLINDRICAL_SURFACE ( 'NONE', #4823, 0.007874015748031516770 ) ;
#5960 = AXIS2_PLACEMENT_3D ( 'NONE', #5204, #8810, #683 ) ;
#5961 = ADVANCED_FACE ( 'NONE', ( #15336, #13225 ), #2412, .F. ) ;
#5962 = DIRECTION ( 'NONE',  ( -0.8660254037844385966, -0.000000000000000000, -0.5000000000000001110 ) ) ;
#5963 = CYLINDRICAL_SURFACE ( 'NONE', #2609, 0.003937007874015724558 ) ;
#5964 = CARTESIAN_POINT ( 'NONE',  ( -1.580080891953811628, 0.1020406297922293454, -0.07874015748031495954 ) ) ;
#5965 = DIRECTION ( 'NONE',  ( -1.000000000000000000, 0.000000000000000000, 0.000000000000000000 ) ) ;
#5966 = VERTEX_POINT ( 'NONE', #8222 ) ;
#5967 = DIRECTION ( 'NONE',  ( -0.8660254037844383745, 0.000000000000000000, -0.5000000000000004441 ) ) ;
#5968 = FACE_OUTER_BOUND ( 'NONE', #11742, .T. ) ;
#5969 = DIRECTION ( 'NONE',  ( 0.4999999999999918954, -0.000000000000000000, -0.8660254037844431485 ) ) ;
#5970 = CARTESIAN_POINT ( 'NONE',  ( 0.000000000000000000, 2.165354330708661568, -0.1574803149606299191 ) ) ;
#5971 = ORIENTED_EDGE ( 'NONE', *, *, #6776, .T. ) ;
#5972 = ORIENTED_EDGE ( 'NONE', *, *, #13834, .F. ) ;
#5973 = ORIENTED_EDGE ( 'NONE', *, *, #3802, .T. ) ;
#5974 = EDGE_CURVE ( 'NONE', #14414, #12552, #7262, .T. ) ;
#5975 = ORIENTED_EDGE ( 'NONE', *, *, #13171, .T. ) ;
#5976 = DIRECTION ( 'NONE',  ( -0.000000000000000000, -1.000000000000000000, -0.000000000000000000 ) ) ;
#5977 = ADVANCED_FACE ( 'NONE', ( #7031 ), #1313, .F. ) ;
#5978 = CARTESIAN_POINT ( 'NONE',  ( 0.000000000000000000, 0.3070866141732283561, 0.000000000000000000 ) ) ;
#5979 = DIRECTION ( 'NONE',  ( -0.5000000000000001110, -0.000000000000000000, -0.8660254037844385966 ) ) ;
#5980 = DIRECTION ( 'NONE',  ( 0.7118260687460290503, 0.5695655044020491165, -0.4109729724067176515 ) ) ;
#5981 = EDGE_CURVE ( 'NONE', #5876, #12044, #143, .T. ) ;
#5982 = DIRECTION ( 'NONE',  ( -0.8660254037844398178, 0.000000000000000000, 0.4999999999999979461 ) ) ;
#5983 = CARTESIAN_POINT ( 'NONE',  ( 0.1023622047244639455, -0.4921259842519685179, -0.5870514566507987197 ) ) ;
#5984 = DIRECTION ( 'NONE',  ( 0.000000000000000000, 1.000000000000000000, 0.000000000000000000 ) ) ;
#5985 = FACE_OUTER_BOUND ( 'NONE', #11904, .T. ) ;
#5986 = APPLICATION_CONTEXT ( 'automotive_design' ) ;
#5987 = ADVANCED_FACE ( 'NONE', ( #7103 ), #9397, .T. ) ;
#5988 = CARTESIAN_POINT ( 'NONE',  ( -1.407046561513447758, -0.03370566694352346293, 0.04739997601650549480 ) ) ;
#5989 = DIRECTION ( 'NONE',  ( 0.000000000000000000, -1.000000000000000000, 0.000000000000000000 ) ) ;
#5990 = ORIENTED_EDGE ( 'NONE', *, *, #4050, .F. ) ;
#5991 = ORIENTED_EDGE ( 'NONE', *, *, #7982, .T. ) ;
#5992 = ORIENTED_EDGE ( 'NONE', *, *, #3524, .T. ) ;
#5993 = ORIENTED_EDGE ( 'NONE', *, *, #988, .F. ) ;
#5994 = DIRECTION ( 'NONE',  ( 1.000000000000000000, 0.000000000000000000, 0.000000000000000000 ) ) ;
#5995 = DIRECTION ( 'NONE',  ( -0.000000000000000000, -0.000000000000000000, -1.000000000000000000 ) ) ;
#5996 = EDGE_CURVE ( 'NONE', #13507, #4728, #4634, .T. ) ;
#5997 = DIRECTION ( 'NONE',  ( -1.000000000000000000, -0.000000000000000000, -0.000000000000000000 ) ) ;
#5998 = DIRECTION ( 'NONE',  ( -1.224646799147343593E-16, 0.000000000000000000, -1.000000000000000000 ) ) ;
#5999 = B_SPLINE_CURVE_WITH_KNOTS ( 'NONE', 3,
 ( #5706, #15206, #14023, #10425, #5628, #4536, #2339, #3286, #11588, #11923, #12772, #2030, #10497, #15354, #9248, #8233, #861, #8057, #1025, #5855, #9318, #12842, #5775, #4385, #2112, #10568, #6889, #4617, #13072, #11683, #2200, #5943, #6974, #6797, #15116, #953 ),
 .UNSPECIFIED., .F., .F.,
 ( 4, 2, 2, 2, 2, 2, 2, 2, 2, 2, 2, 2, 2, 2, 2, 2, 2, 4 ),
 ( 0.0006039794861555876143, 0.001506811385715726981, 0.002409643285275866239, 0.003312475184836005931, 0.004215307084396146056, 0.005118138983956285748, 0.006020970883516425440, 0.006923802783076565999, 0.007375218732856640182, 0.007826634682636715232, 0.008729466582196863597, 0.009632298481757010228, 0.01053513038131715859, 0.01143796228087730696, 0.01234079418043745706, 0.01324362607999760716, 0.01414645797955775379, 0.01504928987911790389 ),
 .UNSPECIFIED. ) ;
#6000 = ORIENTED_EDGE ( 'NONE', *, *, #3723, .F. ) ;
#6001 = PRESENTATION_STYLE_ASSIGNMENT (( #14405 ) ) ;
#6002 = EDGE_CURVE ( 'NONE', #11019, #2631, #6617, .T. ) ;
#6003 = DIRECTION ( 'NONE',  ( 0.000000000000000000, 0.000000000000000000, -1.000000000000000000 ) ) ;
#6004 = CARTESIAN_POINT ( 'NONE',  ( -0.1181102362204724532, 2.637795275590551825, -0.03937007874015747977 ) ) ;
#6005 = VERTEX_POINT ( 'NONE', #4915 ) ;
#6006 = EDGE_LOOP ( 'NONE', ( #13197, #13788, #9904, #3715 ) ) ;
#6007 = VERTEX_POINT ( 'NONE', #14403 ) ;
#6008 = DIRECTION ( 'NONE',  ( 0.5000000000000035527, 0.000000000000000000, -0.8660254037844365982 ) ) ;
#6009 = CARTESIAN_POINT ( 'NONE',  ( -1.596214514379725946, 0.1135332894431583389, 0.07535569387264980101 ) ) ;
#6010 = DIRECTION ( 'NONE',  ( 0.000000000000000000, 0.000000000000000000, -1.000000000000000000 ) ) ;
#6011 = DIRECTION ( 'NONE',  ( -0.5000000000000008882, 0.000000000000000000, 0.8660254037844380415 ) ) ;
#6012 = LINE ( 'NONE', #7208, #10833 ) ;
#6013 = CARTESIAN_POINT ( 'NONE',  ( -0.1574803149606299191, -0.09448818897637796532, -0.5909884645248143498 ) ) ;
#6014 = CARTESIAN_POINT ( 'NONE',  ( -1.951076232067097349, -2.792370830351091904, 0.1761340083271971391 ) ) ;
#6015 = ORIENTED_EDGE ( 'NONE', *, *, #12323, .F. ) ;
#6016 = CARTESIAN_POINT ( 'NONE',  ( -0.7205731843802207770, 1.190944881889763884, 0.4842140986486909715 ) ) ;
#6017 = DIRECTION ( 'NONE',  ( 0.000000000000000000, 2.212657494868377674E-16, -1.000000000000000000 ) ) ;
#6018 = CARTESIAN_POINT ( 'NONE',  ( -0.6523822077042805700, 1.190944881889763884, 0.4448440199085330615 ) ) ;
#6019 = VERTEX_POINT ( 'NONE', #13060 ) ;
#6020 = VERTEX_POINT ( 'NONE', #14172 ) ;
#6021 = EDGE_LOOP ( 'NONE', ( #11258, #9148, #8614, #14306 ) ) ;
#6022 = CARTESIAN_POINT ( 'NONE',  ( 0.1618514667033794652, -0.1023622047244094474, 0.2161887458866224576 ) ) ;
#6023 = DIRECTION ( 'NONE',  ( -0.5000000000000001110, 0.000000000000000000, 0.8660254037844385966 ) ) ;
#6024 = CARTESIAN_POINT ( 'NONE',  ( -1.398374251180654060, -0.02596405602755174485, 0.07123060654724291951 ) ) ;
#6025 = DIRECTION ( 'NONE',  ( -0.4999999999999966693, 0.000000000000000000, 0.8660254037844405950 ) ) ;
#6026 = ITEM_DEFINED_TRANSFORMATION ( 'NONE', 'NONE', #6351,  #11481 ) ;
#6027 = CYLINDRICAL_SURFACE ( 'NONE', #7681, 1.865354330708661745 ) ;
#6028 = DIRECTION ( 'NONE',  ( 1.000000000000000000, -0.000000000000000000, 1.224646799147353207E-16 ) ) ;
#6029 = EDGE_LOOP ( 'NONE', ( #5488, #11387, #4900, #6551 ) ) ;
#6030 = ADVANCED_FACE ( 'NONE', ( #9708 ), #8901, .T. ) ;
#6031 = CARTESIAN_POINT ( 'NONE',  ( -1.595687817112585005, 0.1142625427333565924, -0.07194693897044758535 ) ) ;
#6032 = DIRECTION ( 'NONE',  ( -0.8660254037844383745, 0.000000000000000000, -0.5000000000000004441 ) ) ;
#6033 = CARTESIAN_POINT ( 'NONE',  ( -0.06154672136187318982, -0.1666784585780658190, 0.05764611276129245204 ) ) ;
#6034 = ADVANCED_FACE ( 'NONE', ( #3581 ), #1902, .T. ) ;
#6035 = DIRECTION ( 'NONE',  ( 1.000000000000000000, 0.000000000000000000, 1.224646799147353207E-16 ) ) ;
#6036 = VERTEX_POINT ( 'NONE', #10787 ) ;
#6037 = ADVANCED_FACE ( 'NONE', ( #9624 ), #3659, .T. ) ;
#6038 = ORIENTED_EDGE ( 'NONE', *, *, #14685, .F. ) ;
#6039 = EDGE_LOOP ( 'NONE', ( #9081, #14990, #12635, #676 ) ) ;
#6040 = ORIENTED_EDGE ( 'NONE', *, *, #12425, .T. ) ;
#6041 = CARTESIAN_POINT ( 'NONE',  ( -0.05905511811023622659, 1.190944881889763884, -0.7874015748031497619 ) ) ;
#6042 = DIRECTION ( 'NONE',  ( 0.000000000000000000, 0.000000000000000000, 1.000000000000000000 ) ) ;
#6043 = DIRECTION ( 'NONE',  ( -0.5000000000000001110, -0.000000000000000000, 0.8660254037844385966 ) ) ;
#6044 = CARTESIAN_POINT ( 'NONE',  ( 0.1023622047239132887, 35.52269057326157053, -0.4190977005993519189 ) ) ;
#6045 = CARTESIAN_POINT ( 'NONE',  ( 0.000000000000000000, 0.000000000000000000, -0.5905511811023621549 ) ) ;
#6046 = CARTESIAN_POINT ( 'NONE',  ( 0.6864776960422567242, 1.338582677165354395, 0.4645290592786021633 ) ) ;
#6047 = ADVANCED_FACE ( 'NONE', ( #8446 ), #12412, .T. ) ;
#6048 = DIRECTION ( 'NONE',  ( 0.000000000000000000, 0.000000000000000000, 1.000000000000000000 ) ) ;
#6049 = DIRECTION ( 'NONE',  ( -0.000000000000000000, 1.000000000000000000, 0.000000000000000000 ) ) ;
#6050 = CARTESIAN_POINT ( 'NONE',  ( 0.3512416941306070739, -0.2952755905511811330, 0.3164411144501581563 ) ) ;
#6051 = EDGE_CURVE ( 'NONE', #12320, #6775, #2186, .T. ) ;
#6052 = CARTESIAN_POINT ( 'NONE',  ( -0.06692913385815726923, -0.2952755905511811330, -0.4624047872104674606 ) ) ;
#6053 = DIRECTION ( 'NONE',  ( 0.000000000000000000, 1.000000000000000000, 0.000000000000000000 ) ) ;
#6054 = ORIENTED_EDGE ( 'NONE', *, *, #7223, .T. ) ;
#6055 = EDGE_CURVE ( 'NONE', #11857, #10793, #11651, .T. ) ;
#6056 = ORIENTED_EDGE ( 'NONE', *, *, #5394, .T. ) ;
#6057 = AXIS2_PLACEMENT_3D ( 'NONE', #11013, #13370, #3809 ) ;
#6058 = EDGE_LOOP ( 'NONE', ( #4680, #2541, #8484, #12066 ) ) ;
#6059 = CARTESIAN_POINT ( 'NONE',  ( 0.06692913385832208184, -0.2952755905511811330, -0.3757906139821208247 ) ) ;
#6060 = LINE ( 'NONE', #3667, #1472 ) ;
#6061 = LINE ( 'NONE', #8353, #5935 ) ;
#6062 = CARTESIAN_POINT ( 'NONE',  ( 0.3294846884549027521, -0.2952755905511811330, 0.2675111804726952314 ) ) ;
#6063 = CARTESIAN_POINT ( 'NONE',  ( -0.4606299212598433113, -0.1023622047244094474, 0.3841425019411278674 ) ) ;
#6064 = AXIS2_PLACEMENT_3D ( 'NONE', #4482, #9264, #11700 ) ;
#6065 = VECTOR ( 'NONE', #1839, 39.37007874015748143 ) ;
#6066 = CARTESIAN_POINT ( 'NONE',  ( 0.000000000000000000, 2.637795275590551825, 0.03937007874015747977 ) ) ;
#6067 = AXIS2_PLACEMENT_3D ( 'NONE', #4748, #11804, #10623 ) ;
#6068 = CARTESIAN_POINT ( 'NONE',  ( -2.184126211765464287, -1.725292181286280258, -0.08417626406393655114 ) ) ;
#6069 = LINE ( 'NONE', #7265, #3901 ) ;
#6070 = AXIS2_PLACEMENT_3D ( 'NONE', #13850, #1000, #10093 ) ;
#6071 = EDGE_LOOP ( 'NONE', ( #3318, #4225, #1270, #4421 ) ) ;
#6072 = ORIENTED_EDGE ( 'NONE', *, *, #6478, .F. ) ;
#6073 = EDGE_CURVE ( 'NONE', #4286, #4739, #13284, .T. ) ;
#6074 = ORIENTED_EDGE ( 'NONE', *, *, #12271, .T. ) ;
#6075 = AXIS2_PLACEMENT_3D ( 'NONE', #5919, #7095, #14310 ) ;
#6076 = CIRCLE ( 'NONE', #5083, 0.003937007874015758385 ) ;
#6077 = DIRECTION ( 'NONE',  ( -0.5000000000000003331, -0.000000000000000000, 0.8660254037844387076 ) ) ;
#6078 = AXIS2_PLACEMENT_3D ( 'NONE', #14269, #15285, #5869 ) ;
#6079 = ADVANCED_FACE ( 'NONE', ( #14784 ), #6885, .T. ) ;
#6080 = AXIS2_PLACEMENT_3D ( 'NONE', #6334, #6423, #5016 ) ;
#6081 = LINE ( 'NONE', #80, #12661 ) ;
#6082 = PLANE ( 'NONE',  #8615 ) ;
#6083 = CARTESIAN_POINT ( 'NONE',  ( -0.06425120930260366792, -0.1863186860285575008, -0.03845354371037630614 ) ) ;
#6084 = FACE_BOUND ( 'NONE', #10662, .T. ) ;
#6085 = DIRECTION ( 'NONE',  ( -1.000000000000000000, -0.000000000000000000, -0.000000000000000000 ) ) ;
#6086 = CARTESIAN_POINT ( 'NONE',  ( -1.899889809402484087, -2.871954297241456455, 0.1472027794511626131 ) ) ;
#6087 = ORIENTED_EDGE ( 'NONE', *, *, #14812, .T. ) ;
#6088 = CARTESIAN_POINT ( 'NONE',  ( -1.962446787563433270, -2.889798350705808705, 0.1130053219567358630 ) ) ;
#6089 = AXIS2_PLACEMENT_3D ( 'NONE', #7310, #214, #5031 ) ;
#6090 = DIRECTION ( 'NONE',  ( 0.000000000000000000, -1.000000000000000000, 0.000000000000000000 ) ) ;
#6091 = ORIENTED_EDGE ( 'NONE', *, *, #13678, .F. ) ;
#6092 = VECTOR ( 'NONE', #9826, 39.37007874015748143 ) ;
#6093 = ORIENTED_EDGE ( 'NONE', *, *, #4067, .T. ) ;
#6094 = CIRCLE ( 'NONE', #1606, 0.01968503937007875376 ) ;
#6095 = CIRCLE ( 'NONE', #6338, 0.01968503937007875723 ) ;
#6096 = AXIS2_PLACEMENT_3D ( 'NONE', #14693, #4021, #11384 ) ;
#6097 = ORIENTED_EDGE ( 'NONE', *, *, #12419, .F. ) ;
#6098 = CARTESIAN_POINT ( 'NONE',  ( -0.5860051159906336515, -0.003937007874015747977, 0.1591122789105256785 ) ) ;
#6099 = PRODUCT_DEFINITION ( 'UNKNOWN', '', #6856, #11442 ) ;
#6100 = CARTESIAN_POINT ( 'NONE',  ( 1.220472440944881720, 4.092325622859527280E-16, -0.02559055118110236185 ) ) ;
#6101 = AXIS2_PLACEMENT_3D ( 'NONE', #15300, #15383, #12731 ) ;
#6102 = AXIS2_PLACEMENT_3D ( 'NONE', #4361, #4448, #15258 ) ;
#6103 = AXIS2_PLACEMENT_3D ( 'NONE', #14468, #284, #7312 ) ;
#6104 = AXIS2_PLACEMENT_3D ( 'NONE', #9506, #14273, #3538 ) ;
#6105 = CARTESIAN_POINT ( 'NONE',  ( 0.3294846884549027521, -0.2952755905511811330, 0.2675111804726952314 ) ) ;
#6106 = DIRECTION ( 'NONE',  ( -6.505213034913010038E-15, 0.000000000000000000, -1.000000000000000000 ) ) ;
#6107 = CONTEXT_DEPENDENT_SHAPE_REPRESENTATION ( #14221, #6907 ) ;
#6108 = DIRECTION ( 'NONE',  ( -0.4999999999999919509, 0.000000000000000000, 0.8660254037844432595 ) ) ;
#6109 = VECTOR ( 'NONE', #11764, 39.37007874015748854 ) ;
#6110 = CARTESIAN_POINT ( 'NONE',  ( 0.4788739157331329266, -0.4881889763779528324, 0.3514880584999470203 ) ) ;
#6111 = ORIENTED_EDGE ( 'NONE', *, *, #10813, .T. ) ;
#6112 = CARTESIAN_POINT ( 'NONE',  ( -1.579560462701998569, 0.1027931347612302260, -0.07190453453446270238 ) ) ;
#6113 = DIRECTION ( 'NONE',  ( -0.000000000000000000, -1.000000000000000000, -0.000000000000000000 ) ) ;
#6114 = CARTESIAN_POINT ( 'NONE',  ( 0.000000000000000000, 0.04724409448818898960, 0.000000000000000000 ) ) ;
#6115 = AXIS2_PLACEMENT_3D ( 'NONE', #6066, #14315, #14249 ) ;
#6116 = CIRCLE ( 'NONE', #14899, 0.04330708661417329020 ) ;
#6117 = VECTOR ( 'NONE', #7039, 39.37007874015748143 ) ;
#6118 = EDGE_LOOP ( 'NONE', ( #164, #13769, #8211, #1143 ) ) ;
#6119 = EDGE_LOOP ( 'NONE', ( #2296, #1973, #2060 ) ) ;
#6120 = ORIENTED_EDGE ( 'NONE', *, *, #7495, .T. ) ;
#6121 = CIRCLE ( 'NONE', #13399, 0.1279527559055117780 ) ;
#6122 = ORIENTED_EDGE ( 'NONE', *, *, #2782, .F. ) ;
#6123 = EDGE_CURVE ( 'NONE', #9010, #2747, #11917, .T. ) ;
#6124 = DIRECTION ( 'NONE',  ( 1.000000000000000000, 0.000000000000000000, 0.000000000000000000 ) ) ;
#6125 = ADVANCED_FACE ( 'NONE', ( #9848 ), #1705, .F. ) ;
#6126 = FACE_OUTER_BOUND ( 'NONE', #13479, .T. ) ;
#6127 = DIRECTION ( 'NONE',  ( 0.8660254037844405950, -0.000000000000000000, -0.4999999999999967804 ) ) ;
#6128 = DIRECTION ( 'NONE',  ( -0.4932581959314707443, 0.8219459448134281976, 0.2847827522010268342 ) ) ;
#6129 = AXIS2_PLACEMENT_3D ( 'NONE', #5209, #1622, #14547 ) ;
#6130 = CARTESIAN_POINT ( 'NONE',  ( 0.000000000000000000, 0.3149606299212598381, 0.000000000000000000 ) ) ;
#6131 = AXIS2_PLACEMENT_3D ( 'NONE', #1177, #5930, #6 ) ;
#6132 = CARTESIAN_POINT ( 'NONE',  ( -0.02641567992992046449, 0.1724028871747071145, 1.853431881210122409E-17 ) ) ;
#6133 = AXIS2_PLACEMENT_3D ( 'NONE', #12862, #13970, #15140 ) ;
#6134 = EDGE_CURVE ( 'NONE', #238, #7658, #14632, .T. ) ;
#6135 = CARTESIAN_POINT ( 'NONE',  ( -1.431036756819011213, -0.02829858486107871343, 0.08366141732283458032 ) ) ;
#6136 = FACE_BOUND ( 'NONE', #7836, .T. ) ;
#6137 = CIRCLE ( 'NONE', #11405, 0.01968503937007872254 ) ;
#6138 = B_SPLINE_CURVE_WITH_KNOTS ( 'NONE', 3,
 ( #5068, #89, #4851, #9654, #3693, #14430, #8471, #12068, #6488, #13626 ),
 .UNSPECIFIED., .F., .F.,
 ( 4, 2, 2, 2, 4 ),
 ( 0.000000000000000000, 0.0006582318843486420663, 0.001316463768697284133, 0.001974695653045926199, 0.002632927537394568265 ),
 .UNSPECIFIED. ) ;
#6139 = CARTESIAN_POINT ( 'NONE',  ( -1.417126644544185021, -0.04224944786056485102, 0.06861491064343343271 ) ) ;
#6140 = CARTESIAN_POINT ( 'NONE',  ( -0.03346456692910660530, -0.4921259842519685179, -0.05796233017450189845 ) ) ;
#6141 = ORIENTED_EDGE ( 'NONE', *, *, #13073, .F. ) ;
#6142 = AXIS2_PLACEMENT_3D ( 'NONE', #14041, #11608, #7933 ) ;
#6143 = ORIENTED_EDGE ( 'NONE', *, *, #4526, .T. ) ;
#6144 = EDGE_LOOP ( 'NONE', ( #15065, #10824, #5917, #7734, #5450, #2320 ) ) ;
#6145 = ADVANCED_FACE ( 'NONE', ( #7328 ), #9779, .F. ) ;
#6146 = AXIS2_PLACEMENT_3D ( 'NONE', #9272, #4490, #9514 ) ;
#6147 = EDGE_CURVE ( 'NONE', #3165, #12754, #14664, .T. ) ;
#6148 = B_SPLINE_CURVE_WITH_KNOTS ( 'NONE', 3,
 ( #14786, #466, #14949, #7881, #6612, #690 ),
 .UNSPECIFIED., .F., .F.,
 ( 4, 2, 4 ),
 ( 0.000000000000000000, 0.01440388436194932689, 0.02880776872389865378 ),
 .UNSPECIFIED. ) ;
#6149 = CARTESIAN_POINT ( 'NONE',  ( 0.4572203724260462399, -0.09842519685039372024, 0.3821739980041199969 ) ) ;
#6150 = DIRECTION ( 'NONE',  ( -0.000000000000000000, -0.000000000000000000, 1.000000000000000000 ) ) ;
#6151 = DIRECTION ( 'NONE',  ( 1.060575238724906792E-16, 1.000000000000000000, 6.123233995736766036E-17 ) ) ;
#6152 = ADVANCED_FACE ( 'NONE', ( #4038 ), #6465, .F. ) ;
#6153 = DIRECTION ( 'NONE',  ( 0.8660254037844365982, -0.000000000000000000, 0.5000000000000035527 ) ) ;
#6154 = VECTOR ( 'NONE', #1761, 39.37007874015748143 ) ;
#6155 = DIRECTION ( 'NONE',  ( -1.000000000000000000, -0.000000000000000000, 0.000000000000000000 ) ) ;
#6156 =( NAMED_UNIT ( * ) PLANE_ANGLE_UNIT ( ) SI_UNIT ( $, .RADIAN. ) );
#6157 = CARTESIAN_POINT ( 'NONE',  ( -0.1638199706403874467, -0.4881889763779528324, 0.2127791970528254695 ) ) ;
#6158 = DIRECTION ( 'NONE',  ( -0.000000000000000000, -1.000000000000000000, -0.000000000000000000 ) ) ;
#6159 = AXIS2_PLACEMENT_3D ( 'NONE', #9324, #3377, #8157 ) ;
#6160 = ORIENTED_EDGE ( 'NONE', *, *, #14986, .T. ) ;
#6161 = ORIENTED_EDGE ( 'NONE', *, *, #14605, .T. ) ;
#6162 = ORIENTED_EDGE ( 'NONE', *, *, #7283, .T. ) ;
#6163 = ORIENTED_EDGE ( 'NONE', *, *, #15276, .F. ) ;
#6164 = ORIENTED_EDGE ( 'NONE', *, *, #2513, .F. ) ;
#6165 = AXIS2_PLACEMENT_3D ( 'NONE', #4305, #6572, #6429 ) ;
#6166 = EDGE_CURVE ( 'NONE', #5839, #3335, #8585, .T. ) ;
#6167 = CARTESIAN_POINT ( 'NONE',  ( -1.992382107315058271, -2.749515453455440905, 0.1756903148397124803 ) ) ;
#6168 = AXIS2_PLACEMENT_3D ( 'NONE', #11343, #13475, #1558 ) ;
#6169 = CARTESIAN_POINT ( 'NONE',  ( 0.000000000000000000, 0.003937007874015749712, -0.03937007874015751446 ) ) ;
#6170 = EDGE_CURVE ( 'NONE', #11777, #10892, #5639, .T. ) ;
#6171 = DIRECTION ( 'NONE',  ( -0.5984233124757303290, -0.8011800915434521553, 0.000000000000000000 ) ) ;
#6172 = CARTESIAN_POINT ( 'NONE',  ( 0.2393297813660762718, -0.4921259842519685179, 0.06089400679746260342 ) ) ;
#6173 = CARTESIAN_POINT ( 'NONE',  ( -1.889963351875279196, -2.896989719539225572, -0.08666351837760270793 ) ) ;
#6174 = EDGE_LOOP ( 'NONE', ( #11197, #12222, #5095, #15196 ) ) ;
#6175 = CARTESIAN_POINT ( 'NONE',  ( -2.010991777528384095, -2.758467574604078543, -0.1561691687464109024 ) ) ;
#6176 = CARTESIAN_POINT ( 'NONE',  ( 0.000000000000000000, 0.07480314960629921850, 0.04330708661417326938 ) ) ;
#6177 = VERTEX_POINT ( 'NONE', #3977 ) ;
#6178 = EDGE_CURVE ( 'NONE', #11619, #10362, #7490, .T. ) ;
#6179 = EDGE_LOOP ( 'NONE', ( #4987, #13989, #8754, #9075 ) ) ;
#6180 = CIRCLE ( 'NONE', #11975, 0.003937007874015724558 ) ;
#6181 = EDGE_LOOP ( 'NONE', ( #4936, #11118, #74, #10205 ) ) ;
#6182 = DIRECTION ( 'NONE',  ( 0.000000000000000000, 1.000000000000000000, 0.000000000000000000 ) ) ;
#6183 = AXIS2_PLACEMENT_3D ( 'NONE', #7722, #4115, #10001 ) ;
#6184 =( REPRESENTATION_RELATIONSHIP ('NONE','NONE', #8904, #7785 ) REPRESENTATION_RELATIONSHIP_WITH_TRANSFORMATION ( #2516 )SHAPE_REPRESENTATION_RELATIONSHIP( ) );
#6185 = CARTESIAN_POINT ( 'NONE',  ( 1.928577636452524610E-17, 2.165354330708661568, 0.1574803149606299191 ) ) ;
#6186 = LINE ( 'NONE', #14670, #13862 ) ;
#6187 = CONTEXT_DEPENDENT_SHAPE_REPRESENTATION ( #4289, #11531 ) ;
#6188 = FACE_OUTER_BOUND ( 'NONE', #6518, .T. ) ;
#6189 = AXIS2_PLACEMENT_3D ( 'NONE', #15050, #420, #15449 ) ;
#6190 = DIRECTION ( 'NONE',  ( -0.000000000000000000, -1.734723475976817823E-14, -1.000000000000000000 ) ) ;
#6191 = CARTESIAN_POINT ( 'NONE',  ( -0.03044903239804774148, 0.1717056406757088149, -0.01152843233334087045 ) ) ;
#6192 = EDGE_LOOP ( 'NONE', ( #12257, #7802, #10182, #10306 ) ) ;
#6193 = CARTESIAN_POINT ( 'NONE',  ( -0.000000000000000000, -0.09842519685039370636, -0.5870514566507987197 ) ) ;
#6194 = FACE_OUTER_BOUND ( 'NONE', #4480, .T. ) ;
#6195 = CARTESIAN_POINT ( 'NONE',  ( -0.03747986570939449563, -0.1642921853714506830, 0.04794034192644637538 ) ) ;
#6196 = EDGE_CURVE ( 'NONE', #6434, #14775, #14419, .T. ) ;
#6197 = DIRECTION ( 'NONE',  ( 0.000000000000000000, 0.000000000000000000, 1.000000000000000000 ) ) ;
#6198 = CIRCLE ( 'NONE', #1467, 0.1476377952755906220 ) ;
#6199 = ORIENTED_EDGE ( 'NONE', *, *, #894, .T. ) ;
#6200 = VERTEX_POINT ( 'NONE', #12214 ) ;
#6201 = ORIENTED_EDGE ( 'NONE', *, *, #13638, .F. ) ;
#6202 = AXIS2_PLACEMENT_3D ( 'NONE', #14712, #3972, #10939 ) ;
#6203 = ORIENTED_EDGE ( 'NONE', *, *, #12887, .T. ) ;
#6204 = FACE_OUTER_BOUND ( 'NONE', #2990, .T. ) ;
#6205 = DIRECTION ( 'NONE',  ( 0.000000000000000000, 0.000000000000000000, -1.000000000000000000 ) ) ;
#6206 = CARTESIAN_POINT ( 'NONE',  ( 0.5860051159906326523, -0.003937007874015747977, 0.1591122789105293422 ) ) ;
#6207 = CARTESIAN_POINT ( 'NONE',  ( -0.4591888763630546655, -0.4881889763779528324, 0.3787644491703233141 ) ) ;
#6208 = CARTESIAN_POINT ( 'NONE',  ( 0.4436579168042673049, 35.52269057326158475, 0.06975734811352231335 ) ) ;
#6209 = CARTESIAN_POINT ( 'NONE',  ( -1.419615703680148000, -0.01226548409420231273, 0.07874015748031495954 ) ) ;
#6210 = CARTESIAN_POINT ( 'NONE',  ( -0.5484644751328247025, 0.000000000000000000, 0.2393730054594876144 ) ) ;
#6211 = FACE_OUTER_BOUND ( 'NONE', #10932, .T. ) ;
#6212 = CARTESIAN_POINT ( 'NONE',  ( -1.580259682937499965, 0.1018956540319304049, 0.04477369844320259334 ) ) ;
#6213 = CARTESIAN_POINT ( 'NONE',  ( -2.100501784635051550, -1.630597114118274460, -0.08366141732283423338 ) ) ;
#6214 = DIRECTION ( 'NONE',  ( 1.000000000000000000, 0.000000000000000000, -1.224646799147353207E-16 ) ) ;
#6215 = ORIENTED_EDGE ( 'NONE', *, *, #9977, .T. ) ;
#6216 = ORIENTED_EDGE ( 'NONE', *, *, #12530, .F. ) ;
#6217 = VERTEX_POINT ( 'NONE', #7647 ) ;
#6218 = ADVANCED_FACE ( 'NONE', ( #12436 ), #8147, .T. ) ;
#6219 = DIRECTION ( 'NONE',  ( 0.8660254037844365982, -0.000000000000000000, 0.5000000000000035527 ) ) ;
#6220 = CARTESIAN_POINT ( 'NONE',  ( -1.940380551367184125, -2.944208869897690928, 0.04343028329486892797 ) ) ;
#6221 = LINE ( 'NONE', #1390, #12238 ) ;
#6222 = FACE_OUTER_BOUND ( 'NONE', #13924, .T. ) ;
#6223 = CARTESIAN_POINT ( 'NONE',  ( -1.591501945092674841, 0.08600752902535285793, 0.07874015748031495954 ) ) ;
#6224 = CARTESIAN_POINT ( 'NONE',  ( 0.000000000000000000, 0.5905511811023621549, 0.000000000000000000 ) ) ;
#6225 = CARTESIAN_POINT ( 'NONE',  ( 0.000000000000000000, 0.03149606299212599769, 0.000000000000000000 ) ) ;
#6226 = ADVANCED_FACE ( 'NONE', ( #11014, #8750 ), #295, .T. ) ;
#6227 = LINE ( 'NONE', #156, #2322 ) ;
#6228 = DIRECTION ( 'NONE',  ( 8.673617379884028076E-17, -1.000000000000000000, 0.000000000000000000 ) ) ;
#6229 = EDGE_CURVE ( 'NONE', #5785, #9354, #5889, .T. ) ;
#6230 = ORIENTED_EDGE ( 'NONE', *, *, #15337, .T. ) ;
#6231 = ORIENTED_EDGE ( 'NONE', *, *, #4999, .F. ) ;
#6232 = ORIENTED_EDGE ( 'NONE', *, *, #13183, .T. ) ;
#6233 = ORIENTED_EDGE ( 'NONE', *, *, #7579, .F. ) ;
#6234 = EDGE_CURVE ( 'NONE', #15326, #11438, #598, .T. ) ;
#6235 = ORIENTED_EDGE ( 'NONE', *, *, #10373, .F. ) ;
#6236 = CARTESIAN_POINT ( 'NONE',  ( -1.414139891776604818, -0.03961000916150922424, -0.05844465851538532125 ) ) ;
#6237 = CARTESIAN_POINT ( 'NONE',  ( 0.5450083523900213223, 1.338582677165354395, 0.2464697422870268384 ) ) ;
#6238 = DIRECTION ( 'NONE',  ( -0.000000000000000000, -0.000000000000000000, -1.000000000000000000 ) ) ;
#6239 = DIRECTION ( 'NONE',  ( -0.8660254037844431485, 0.000000000000000000, -0.4999999999999918954 ) ) ;
#6240 = CARTESIAN_POINT ( 'NONE',  ( 0.05905511811029064834, -0.09448818897637796532, -0.5870514566507987197 ) ) ;
#6241 = CARTESIAN_POINT ( 'NONE',  ( -1.891382748001904535, -2.893416385725415374, 0.09138685817115685395 ) ) ;
#6242 = ORIENTED_EDGE ( 'NONE', *, *, #14885, .F. ) ;
#6243 = CARTESIAN_POINT ( 'NONE',  ( -2.176576600059022759, -2.015093358877955154, -0.09005837916855936875 ) ) ;
#6244 = EDGE_CURVE ( 'NONE', #8322, #8022, #1162, .T. ) ;
#6245 = CARTESIAN_POINT ( 'NONE',  ( -0.05905511811023622659, 1.043263280880422528, -0.5946706712680680518 ) ) ;
#6246 = ADVANCED_FACE ( 'NONE', ( #12514 ), #2900, .T. ) ;
#6247 = EDGE_LOOP ( 'NONE', ( #5682, #10991 ) ) ;
#6248 = ORIENTED_EDGE ( 'NONE', *, *, #12230, .T. ) ;
#6249 = ADVANCED_FACE ( 'NONE', ( #10160 ), #4343, .F. ) ;
#6250 = ORIENTED_EDGE ( 'NONE', *, *, #6051, .T. ) ;
#6251 = DIRECTION ( 'NONE',  ( 0.000000000000000000, 0.000000000000000000, 1.000000000000000000 ) ) ;
#6252 = DIRECTION ( 'NONE',  ( 0.000000000000000000, 1.000000000000000000, 0.000000000000000000 ) ) ;
#6253 = DIRECTION ( 'NONE',  ( -0.000000000000000000, 1.000000000000000000, -0.000000000000000000 ) ) ;
#6254 = CARTESIAN_POINT ( 'NONE',  ( -0.03005672326763337773, -0.1816858507396494349, -0.01806077797202005480 ) ) ;
#6255 = ORIENTED_EDGE ( 'NONE', *, *, #11709, .F. ) ;
#6256 = LINE ( 'NONE', #6193, #9942 ) ;
#6257 = DIRECTION ( 'NONE',  ( -0.000000000000000000, 0.000000000000000000, 1.000000000000000000 ) ) ;
#6258 = DIRECTION ( 'NONE',  ( 0.5000000000000041078, -0.000000000000000000, 0.8660254037844363761 ) ) ;
#6259 = CARTESIAN_POINT ( 'NONE',  ( -0.01782267696647954827, -0.1622289191103822581, 0.03095755538600573897 ) ) ;
#6260 = CARTESIAN_POINT ( 'NONE',  ( -0.002500327830562678200, 0.1532658568795227105, 0.000000000000000000 ) ) ;
#6261 = ORIENTED_EDGE ( 'NONE', *, *, #3570, .F. ) ;
#6262 = SHAPE_REPRESENTATION ( 'Housing', ( #11481 ), #7464 ) ;
#6263 = ADVANCED_FACE ( 'NONE', ( #6769 ), #2955, .F. ) ;
#6264 = ORIENTED_EDGE ( 'NONE', *, *, #2802, .F. ) ;
#6265 = ORIENTED_EDGE ( 'NONE', *, *, #11716, .T. ) ;
#6266 = CARTESIAN_POINT ( 'NONE',  ( -0.1023622047242992716, -0.1023622047244094474, -0.2472069366677729363 ) ) ;
#6267 = DIRECTION ( 'NONE',  ( -1.000000000000000000, 0.000000000000000000, 0.000000000000000000 ) ) ;
#6268 = EDGE_CURVE ( 'NONE', #3814, #426, #11491, .T. ) ;
#6269 = EDGE_CURVE ( 'NONE', #10807, #5518, #14912, .T. ) ;
#6270 = CARTESIAN_POINT ( 'NONE',  ( -2.080881322745466555, -1.632190302820504257, 0.1033464566929129802 ) ) ;
#6271 = DIRECTION ( 'NONE',  ( -8.673617379884087537E-15, -1.000000000000000000, 0.000000000000000000 ) ) ;
#6272 = DIRECTION ( 'NONE',  ( 0.5000000000000046629, 4.518412553833339729E-17, 0.8660254037844359321 ) ) ;
#6273 = FACE_BOUND ( 'NONE', #9945, .T. ) ;
#6274 = CYLINDRICAL_SURFACE ( 'NONE', #14887, 0.5905511811023621549 ) ;
#6275 = DIRECTION ( 'NONE',  ( 0.000000000000000000, 0.000000000000000000, 1.000000000000000000 ) ) ;
#6276 = CARTESIAN_POINT ( 'NONE',  ( 0.06692913385832215123, -0.4881889763779528324, -0.5870514566507987197 ) ) ;
#6277 = CARTESIAN_POINT ( 'NONE',  ( -0.07874015748031543138, -0.1682792322177920907, -0.05905511811023622659 ) ) ;
#6278 = ORIENTED_EDGE ( 'NONE', *, *, #2177, .F. ) ;
#6279 = EDGE_LOOP ( 'NONE', ( #736, #11792, #1651 ) ) ;
#6280 = ORIENTED_EDGE ( 'NONE', *, *, #14890, .F. ) ;
#6281 = PRODUCT_DEFINITION_SHAPE ( 'NONE', 'NONE',  #15476 ) ;
#6282 = PRODUCT_DEFINITION ( 'UNKNOWN', '', #1364, #1269 ) ;
#6283 = LINE ( 'NONE', #1767, #12344 ) ;
#6284 = CARTESIAN_POINT ( 'NONE',  ( -1.946824355069869394, -2.928629402500327661, 0.08439192439263279444 ) ) ;
#6285 = CARTESIAN_POINT ( 'NONE',  ( 0.1657884745773951785, -0.4881889763779528324, 0.2093696482190284258 ) ) ;
#6286 = DIRECTION ( 'NONE',  ( -0.000000000000000000, -0.000000000000000000, -1.000000000000000000 ) ) ;
#6287 = SPHERICAL_SURFACE ( 'NONE', #2332, 0.003937007874015747977 ) ;
#6288 = CARTESIAN_POINT ( 'NONE',  ( 8.630384923125046426E-17, 1.377952755905512028, -0.7007874015748031260 ) ) ;
#6289 = CARTESIAN_POINT ( 'NONE',  ( -0.09061599198715356018, 0.000000000000000000, -0.007444810018878696839 ) ) ;
#6290 = CARTESIAN_POINT ( 'NONE',  ( -1.889903596530551733, -2.897138837246827414, -0.08643254935806948813 ) ) ;
#6291 = DIRECTION ( 'NONE',  ( 0.000000000000000000, -0.000000000000000000, 1.000000000000000000 ) ) ;
#6292 = VERTEX_POINT ( 'NONE', #3027 ) ;
#6293 = VERTEX_POINT ( 'NONE', #7880 ) ;
#6294 = EDGE_LOOP ( 'NONE', ( #5769, #14344, #8085, #4586 ) ) ;
#6295 = EDGE_LOOP ( 'NONE', ( #1732, #4604, #10685, #10324, #12027 ) ) ;
#6296 = EDGE_LOOP ( 'NONE', ( #5470, #5278 ) ) ;
#6297 = CARTESIAN_POINT ( 'NONE',  ( -1.391725923719789426, -0.02262183056853206073, -0.06139678143372313823 ) ) ;
#6298 = EDGE_CURVE ( 'NONE', #10074, #14540, #11344, .T. ) ;
#6299 = DIRECTION ( 'NONE',  ( 0.000000000000000000, 0.000000000000000000, 1.000000000000000000 ) ) ;
#6300 = AXIS2_PLACEMENT_3D ( 'NONE', #8749, #12127, #10859 ) ;
#6301 = ADVANCED_FACE ( 'NONE', ( #5447 ), #15020, .F. ) ;
#6302 = AXIS2_PLACEMENT_3D ( 'NONE', #11317, #11253, #601 ) ;
#6303 = DIRECTION ( 'NONE',  ( 1.000000000000000000, 0.000000000000000000, 3.973232667114492835E-16 ) ) ;
#6304 = DIRECTION ( 'NONE',  ( -0.5000000000000001110, -0.000000000000000000, -0.8660254037844385966 ) ) ;
#6305 = AXIS2_PLACEMENT_3D ( 'NONE', #11194, #3328, #5746 ) ;
#6306 = CARTESIAN_POINT ( 'NONE',  ( 0.4496668909809713455, -0.2952755905511811330, 0.1459636727603555173 ) ) ;
#6307 = CARTESIAN_POINT ( 'NONE',  ( -1.187809996375178034, 0.3305575196843282271, 0.05905511802048958592 ) ) ;
#6308 = CARTESIAN_POINT ( 'NONE',  ( -1.897884506782005376, -2.949473116112335536, 0.01330914593066468560 ) ) ;
#6309 = ORIENTED_EDGE ( 'NONE', *, *, #3679, .F. ) ;
#6310 = FACE_OUTER_BOUND ( 'NONE', #14645, .T. ) ;
#6311 = ADVANCED_FACE ( 'NONE', ( #1932 ), #6697, .T. ) ;
#6312 = FACE_BOUND ( 'NONE', #5006, .T. ) ;
#6313 = DIRECTION ( 'NONE',  ( 0.000000000000000000, 0.000000000000000000, 1.000000000000000000 ) ) ;
#6314 = ORIENTED_EDGE ( 'NONE', *, *, #10953, .F. ) ;
#6315 = EDGE_LOOP ( 'NONE', ( #2789, #13679, #10647, #10511 ) ) ;
#6316 = AXIS2_PLACEMENT_3D ( 'NONE', #6952, #1009, #5757 ) ;
#6317 = AXIS2_PLACEMENT_3D ( 'NONE', #4743, #5979, #3422 ) ;
#6318 = TOROIDAL_SURFACE ( 'NONE', #2092, 0.5826771653543306728, 0.007874015748031495954 ) ;
#6319 = AXIS2_PLACEMENT_3D ( 'NONE', #4236, #5546, #11594 ) ;
#6320 = VERTEX_POINT ( 'NONE', #757 ) ;
#6321 = ADVANCED_FACE ( 'NONE', ( #5515 ), #12747, .T. ) ;
#6322 = EDGE_CURVE ( 'NONE', #2117, #5520, #13403, .T. ) ;
#6323 = B_SPLINE_CURVE_WITH_KNOTS ( 'NONE', 3,
 ( #233, #2724, #1315, #2643, #5138, #12216 ),
 .UNSPECIFIED., .F., .F.,
 ( 4, 2, 4 ),
 ( 0.000000000000000000, 0.0001791382075655866988, 0.0003582764151311733977 ),
 .UNSPECIFIED. ) ;
#6324 = FACE_BOUND ( 'NONE', #14307, .T. ) ;
#6325 = DIRECTION ( 'NONE',  ( -3.973232667114494807E-16, 0.000000000000000000, 1.000000000000000000 ) ) ;
#6326 = CIRCLE ( 'NONE', #3099, 0.003937007874015741038 ) ;
#6327 = CARTESIAN_POINT ( 'NONE',  ( 0.000000000000000000, -0.1023622047244094474, 0.000000000000000000 ) ) ;
#6328 = VECTOR ( 'NONE', #10996, 39.37007874015748143 ) ;
#6329 = CARTESIAN_POINT ( 'NONE',  ( -0.02345217991005641225, -0.1628325660491150295, -0.03705913340085396912 ) ) ;
#6330 = ORIENTED_EDGE ( 'NONE', *, *, #13619, .T. ) ;
#6331 = CARTESIAN_POINT ( 'NONE',  ( -1.969442568012797157, -2.674162197727227408, 0.1468011070627323611 ) ) ;
#6332 = AXIS2_PLACEMENT_3D ( 'NONE', #14232, #47, #7169 ) ;
#6333 = ADVANCED_FACE ( 'NONE', ( #9822 ), #4888, .T. ) ;
#6334 = CARTESIAN_POINT ( 'NONE',  ( 0.4307978335858663188, -0.003937007874015747977, 0.4279391777402732910 ) ) ;
#6335 = AXIS2_PLACEMENT_3D ( 'NONE', #11756, #9482, #14319 ) ;
#6336 = EDGE_CURVE ( 'NONE', #777, #8, #3404, .T. ) ;
#6337 = CARTESIAN_POINT ( 'NONE',  ( -1.181102362204724310, 0.000000000000000000, -0.02559055118110236185 ) ) ;
#6338 = AXIS2_PLACEMENT_3D ( 'NONE', #14461, #9037, #14999 ) ;
#6339 = CARTESIAN_POINT ( 'NONE',  ( -0.01854992166427318900, -0.1800031784444983685, -0.005378007177148339153 ) ) ;
#6340 = DIRECTION ( 'NONE',  ( 0.000000000000000000, -1.000000000000000000, 0.000000000000000000 ) ) ;
#6341 = ORIENTED_EDGE ( 'NONE', *, *, #7804, .F. ) ;
#6343 = ORIENTED_EDGE ( 'NONE', *, *, #9992, .T. ) ;
#6342 = AXIS2_PLACEMENT_3D ( 'NONE', #243, #8694, #8762 ) ;
#6344 = AXIS2_PLACEMENT_3D ( 'NONE', #3117, #834, #3201 ) ;
#6345 = ORIENTED_EDGE ( 'NONE', *, *, #1937, .T. ) ;
#6346 = VECTOR ( 'NONE', #9245, 39.37007874015748143 ) ;
#6347 = CIRCLE ( 'NONE', #9635, 0.03937007874015747977 ) ;
#6348 = DIRECTION ( 'NONE',  ( 0.8660254037844385966, -0.000000000000000000, 0.5000000000000001110 ) ) ;
#6349 = CARTESIAN_POINT ( 'NONE',  ( -0.1022864650139100884, 0.000000000000000000, -1.048351444896847144E-20 ) ) ;
#6350 = VECTOR ( 'NONE', #172, 39.37007874015748143 ) ;
#6351 = AXIS2_PLACEMENT_3D ( 'NONE', #12034, #1294, #2839 ) ;
#6352 = CARTESIAN_POINT ( 'NONE',  ( -1.974924404908016129, -2.653778228660402139, 0.1636761890514014939 ) ) ;
#6353 = CARTESIAN_POINT ( 'NONE',  ( 0.1181102362204724254, 2.440944881889764329, 0.03937007874015747977 ) ) ;
#6354 = CARTESIAN_POINT ( 'NONE',  ( -2.252067189776977073E-14, 35.67284691056339341, -0.2348438967704718217 ) ) ;
#6355 = CARTESIAN_POINT ( 'NONE',  ( -0.1552072824047652788, -0.09448818897637796532, -0.5870514566507987197 ) ) ;
#6356 = CARTESIAN_POINT ( 'NONE',  ( 0.1259842519685039353, 2.440944881889763884, 0.03937007874015747977 ) ) ;
#6357 = DIRECTION ( 'NONE',  ( 1.000000000000000000, -0.000000000000000000, 1.224646799147353207E-16 ) ) ;
#6358 = ADVANCED_FACE ( 'NONE', ( #12183 ), #11142, .F. ) ;
#6359 = DIRECTION ( 'NONE',  ( 0.000000000000000000, -1.000000000000000000, 0.000000000000000000 ) ) ;
#6360 = CIRCLE ( 'NONE', #10128, 0.5984251968503937480 ) ;
#6361 = AXIS2_PLACEMENT_3D ( 'NONE', #5802, #6826, #5729 ) ;
#6362 = TOROIDAL_SURFACE ( 'NONE', #14900, 0.1240157480314959815, 0.003937007874015747977 ) ;
#6363 =( BOUNDED_SURFACE ( )  B_SPLINE_SURFACE ( 3, 2, ( 
 ( #11746, #7025, #4447 ),
 ( #11568, #10403, #6778 ),
 ( #5685, #3511, #9152 ),
 ( #2314, #3200, #15257 ) ),
 .UNSPECIFIED., .F., .F., .T. ) 
 B_SPLINE_SURFACE_WITH_KNOTS ( ( 4, 4 ),
 ( 3, 3 ),
 ( 4.712388980384689674, 5.242505698888894727 ),
 ( 0.000000000000000000, 1.000000000000000000 ),
 .UNSPECIFIED. ) 
 GEOMETRIC_REPRESENTATION_ITEM ( )  RATIONAL_B_SPLINE_SURFACE ( (
 ( 1.000000000000000000, 0.7071067811865471286, 1.000000000000000000),
 ( 1.000000000000000000, 0.7085172298914497180, 1.000000000000000000),
 ( 1.000000000000000000, 0.7099209393058720785, 1.000000000000000000),
 ( 1.000000000000000000, 0.7111298678009152496, 1.000000000000000000) ) ) 
 REPRESENTATION_ITEM ( '' )  SURFACE ( )  );
#6364 = CARTESIAN_POINT ( 'NONE',  ( -0.05905511811023622659, 1.043307086614173373, -0.5955041639236610118 ) ) ;
#6365 = ORIENTED_EDGE ( 'NONE', *, *, #3691, .F. ) ;
#6366 = CIRCLE ( 'NONE', #3141, 0.003937007874015749712 ) ;
#6367 = ORIENTED_EDGE ( 'NONE', *, *, #11214, .T. ) ;
#6368 = EDGE_CURVE ( 'NONE', #12059, #9714, #9907, .T. ) ;
#6369 = DIRECTION ( 'NONE',  ( -0.8660254037844398178, 0.000000000000000000, 0.4999999999999979461 ) ) ;
#6370 = ORIENTED_EDGE ( 'NONE', *, *, #12982, .F. ) ;
#6371 = VERTEX_POINT ( 'NONE', #1449 ) ;
#6372 = AXIS2_PLACEMENT_3D ( 'NONE', #2319, #5926, #12051 ) ;
#6373 = CIRCLE ( 'NONE', #7377, 0.003937007874015749712 ) ;
#6374 = CIRCLE ( 'NONE', #3407, 0.03937007874015751446 ) ;
#6375 = DIRECTION ( 'NONE',  ( -0.8660254037844385966, 0.000000000000000000, 0.5000000000000000000 ) ) ;
#6376 = CARTESIAN_POINT ( 'NONE',  ( -1.955316446157987276, -2.907727917705189125, 0.1149967193102930108 ) ) ;
#6377 = AXIS2_PLACEMENT_3D ( 'NONE', #11012, #1170, #5923 ) ;
#6378 = PLANE ( 'NONE',  #5442 ) ;
#6379 = CARTESIAN_POINT ( 'NONE',  ( -1.996857264586939129, -2.798601985277512139, -0.1754253142013137701 ) ) ;
#6380 = DIRECTION ( 'NONE',  ( 0.000000000000000000, 0.000000000000000000, 1.000000000000000000 ) ) ;
#6381 = CARTESIAN_POINT ( 'NONE',  ( 0.07874015748031494566, 0.1699885096953269725, -0.03937007874015747283 ) ) ;
#6382 = DIRECTION ( 'NONE',  ( -0.000000000000000000, -1.000000000000000000, -0.000000000000000000 ) ) ;
#6383 = DIRECTION ( 'NONE',  ( 0.000000000000000000, 0.000000000000000000, 1.000000000000000000 ) ) ;
#6384 = VECTOR ( 'NONE', #13425, 39.37007874015748143 ) ;
#6385 = MECHANICAL_DESIGN_GEOMETRIC_PRESENTATION_REPRESENTATION (  '', ( #3661 ), #907 ) ;
#6386 = AXIS2_PLACEMENT_3D ( 'NONE', #7240, #8419, #12184 ) ;
#6387 = ORIENTED_EDGE ( 'NONE', *, *, #12419, .T. ) ;
#6388 = EDGE_CURVE ( 'NONE', #4713, #4318, #6631, .T. ) ;
#6389 = VERTEX_POINT ( 'NONE', #2926 ) ;
#6390 = ORIENTED_EDGE ( 'NONE', *, *, #5957, .T. ) ;
#6391 = CIRCLE ( 'NONE', #5398, 0.1476377952755906775 ) ;
#6392 = EDGE_LOOP ( 'NONE', ( #6662, #9729, #7516, #1811 ) ) ;
#6393 = VERTEX_POINT ( 'NONE', #4088 ) ;
#6394 = CARTESIAN_POINT ( 'NONE',  ( -1.399712685227380460, -0.02644324263748139281, -0.07874015748031495954 ) ) ;
#6395 = CARTESIAN_POINT ( 'NONE',  ( 0.1062992125984796032, -0.4881889763779528324, -0.2482618547481154347 ) ) ;
#6396 = AXIS2_PLACEMENT_3D ( 'NONE', #2626, #14537, #9921 ) ;
#6397 = DIRECTION ( 'NONE',  ( -0.8660254037844385966, -0.000000000000000000, 0.5000000000000001110 ) ) ;
#6398 = LINE ( 'NONE', #11191, #3356 ) ;
#6399 = CYLINDRICAL_SURFACE ( 'NONE', #5130, 0.003937007874015724558 ) ;
#6400 = CYLINDRICAL_SURFACE ( 'NONE', #588, 0.03937007874015751446 ) ;
#6401 = CARTESIAN_POINT ( 'NONE',  ( -0.4751993499419962519, 1.346456692913385877, 0.3506226965216301950 ) ) ;
#6402 = CIRCLE ( 'NONE', #7420, 0.003937007874015721089 ) ;
#6403 = CARTESIAN_POINT ( 'NONE',  ( -1.902069599514452536, -2.937971526065610295, -0.06318319403201104467 ) ) ;
#6404 = VERTEX_POINT ( 'NONE', #4017 ) ;
#6405 = CYLINDRICAL_SURFACE ( 'NONE', #5171, 0.003937007874015724558 ) ;
#6406 = DIRECTION ( 'NONE',  ( -0.8011800915434513781, 0.5984233124757313282, 0.000000000000000000 ) ) ;
#6407 = DIRECTION ( 'NONE',  ( -0.000000000000000000, -1.000000000000000000, -0.000000000000000000 ) ) ;
#6408 = EDGE_LOOP ( 'NONE', ( #1924, #14657, #2462, #14473 ) ) ;
#6409 = VERTEX_POINT ( 'NONE', #5180 ) ;
#6410 = ADVANCED_FACE ( 'NONE', ( #11227 ), #13659, .F. ) ;
#6411 = ORIENTED_EDGE ( 'NONE', *, *, #3982, .T. ) ;
#6412 = CIRCLE ( 'NONE', #14197, 0.003937007874015721089 ) ;
#6413 = EDGE_CURVE ( 'NONE', #7977, #13096, #15415, .T. ) ;
#6414 = B_SPLINE_CURVE_WITH_KNOTS ( 'NONE', 3,
 ( #2738, #14738, #174, #10020, #12064, #394 ),
 .UNSPECIFIED., .F., .F.,
 ( 4, 2, 4 ),
 ( 0.000000000000000000, 0.0001791382075655877830, 0.0003582764151311755661 ),
 .UNSPECIFIED. ) ;
#6415 = CARTESIAN_POINT ( 'NONE',  ( -0.7455328141524873997, 1.190944881889763884, 0.3622425942647021779 ) ) ;
#6416 = DIRECTION ( 'NONE',  ( 3.476578583725179813E-16, 0.000000000000000000, -1.000000000000000000 ) ) ;
#6417 = AXIS2_PLACEMENT_3D ( 'NONE', #6240, #6085, #1416 ) ;
#6419 = CIRCLE ( 'NONE', #5432, 0.01968503937007873988 ) ;
#6418 = DIRECTION ( 'NONE',  ( 1.000000000000000000, 1.040834085586083310E-14, 0.000000000000000000 ) ) ;
#6420 = CARTESIAN_POINT ( 'NONE',  ( -0.06972667172716363881, -0.1870117487642863896, -0.03937007824553747509 ) ) ;
#6421 = ORIENTED_EDGE ( 'NONE', *, *, #634, .F. ) ;
#6422 = CARTESIAN_POINT ( 'NONE',  ( -1.181102362204724310, 0.000000000000000000, 0.02559055118110236185 ) ) ;
#6423 = DIRECTION ( 'NONE',  ( -1.000000000000000000, -0.000000000000000000, 3.469446951953635015E-14 ) ) ;
#6424 = DIRECTION ( 'NONE',  ( 0.000000000000000000, 2.212657494868377674E-16, -1.000000000000000000 ) ) ;
#6425 = CIRCLE ( 'NONE', #6673, 0.003937007874015724558 ) ;
#6426 = CARTESIAN_POINT ( 'NONE',  ( -0.4307978335858689833, -0.09448818897637796532, 0.4279391777402706265 ) ) ;
#6427 = DIRECTION ( 'NONE',  ( -4.425882400543264939E-32, 1.000000000000000000, 1.224646799147353207E-16 ) ) ;
#6428 = PRODUCT_DEFINITION_SHAPE ( 'NONE', 'NONE',  #15492 ) ;
#6429 = DIRECTION ( 'NONE',  ( -0.8660254037844383745, 0.000000000000000000, 0.5000000000000004441 ) ) ;
#6430 = ADVANCED_FACE ( 'NONE', ( #9983 ), #7385, .T. ) ;
#6431 = CIRCLE ( 'NONE', #10192, 0.01968503937007873295 ) ;
#6432 = EDGE_CURVE ( 'NONE', #6722, #8823, #3863, .T. ) ;
#6433 = ORIENTED_EDGE ( 'NONE', *, *, #1087, .T. ) ;
#6434 = VERTEX_POINT ( 'NONE', #2692 ) ;
#6435 = ADVANCED_FACE ( 'NONE', ( #7466 ), #3946, .F. ) ;
#6436 = DIRECTION ( 'NONE',  ( 0.000000000000000000, 0.000000000000000000, 1.000000000000000000 ) ) ;
#6437 = DIRECTION ( 'NONE',  ( 0.9967194639908912857, -0.08093398607328357308, 0.000000000000000000 ) ) ;
#6438 = CARTESIAN_POINT ( 'NONE',  ( -2.018751945719120755, -2.567790922178344371, 0.1539137670609011521 ) ) ;
#6439 = CARTESIAN_POINT ( 'NONE',  ( -1.181102362204724310, 0.000000000000000000, 0.02952755905511811330 ) ) ;
#6440 = APPLICATION_PROTOCOL_DEFINITION ( 'draft international standard', 'automotive_design', 1998, #9718 ) ;
#6441 = CARTESIAN_POINT ( 'NONE',  ( -0.02590706759391929112, 0.06931031770563762795, -0.08113392229587841620 ) ) ;
#6442 = DIRECTION ( 'NONE',  ( 0.000000000000000000, -1.000000000000000000, 0.000000000000000000 ) ) ;
#6443 = CARTESIAN_POINT ( 'NONE',  ( -0.6582248459352179060, -0.2952755905511811330, -0.3018834747714004840 ) ) ;
#6444 = CYLINDRICAL_SURFACE ( 'NONE', #10104, 0.003937007874015749712 ) ;
#6445 = LINE ( 'NONE', #576, #8893 ) ;
#6446 = TOROIDAL_SURFACE ( 'NONE', #2461, 0.1614173228346456879, 0.003937007874015747977 ) ;
#6447 = EDGE_CURVE ( 'NONE', #4124, #4812, #5324, .T. ) ;
#6448 = DIRECTION ( 'NONE',  ( 0.5000000000000036637, -0.000000000000000000, 0.8660254037844364872 ) ) ;
#6449 = ORIENTED_EDGE ( 'NONE', *, *, #3555, .T. ) ;
#6450 = CIRCLE ( 'NONE', #2207, 0.003937007874015724558 ) ;
#6451 = EDGE_CURVE ( 'NONE', #6858, #11438, #6901, .T. ) ;
#6452 = EDGE_LOOP ( 'NONE', ( #6161, #11458, #709 ) ) ;
#6453 = VERTEX_POINT ( 'NONE', #10046 ) ;
#6454 = ORIENTED_EDGE ( 'NONE', *, *, #15099, .F. ) ;
#6455 = ADVANCED_FACE ( 'NONE', ( #6204 ), #14827, .T. ) ;
#6456 = EDGE_CURVE ( 'NONE', #14956, #715, #14920, .T. ) ;
#6457 = CIRCLE ( 'NONE', #3968, 0.007874015748031516770 ) ;
#6458 = DIRECTION ( 'NONE',  ( 0.000000000000000000, 1.000000000000000000, 0.000000000000000000 ) ) ;
#6459 = CARTESIAN_POINT ( 'NONE',  ( -1.958647179939665639, -2.899418888633596314, 0.1240863880612434328 ) ) ;
#6460 = LENGTH_MEASURE_WITH_UNIT ( LENGTH_MEASURE( 0.02539999999999999897 ), #9999 );
#6461 = FACE_OUTER_BOUND ( 'NONE', #1030, .T. ) ;
#6462 = ADVANCED_FACE ( 'NONE', ( #8075 ), #13663, .T. ) ;
#6463 = DIRECTION ( 'NONE',  ( 0.4999999999999995004, 0.000000000000000000, 0.8660254037844390407 ) ) ;
#6464 = CARTESIAN_POINT ( 'NONE',  ( -1.607606114292111199, 0.09732815221480034529, -0.08366141732283460808 ) ) ;
#6465 = PLANE ( 'NONE',  #6129 ) ;
#6466 = FACE_OUTER_BOUND ( 'NONE', #15039, .T. ) ;
#6467 = FACE_OUTER_BOUND ( 'NONE', #11955, .T. ) ;
#6468 = DIRECTION ( 'NONE',  ( 0.000000000000000000, 1.000000000000000000, 0.000000000000000000 ) ) ;
#6469 = ORIENTED_EDGE ( 'NONE', *, *, #2996, .F. ) ;
#6470 = EDGE_LOOP ( 'NONE', ( #3696, #6433 ) ) ;
#6471 = ORIENTED_EDGE ( 'NONE', *, *, #8307, .F. ) ;
#6472 = ORIENTED_EDGE ( 'NONE', *, *, #13721, .F. ) ;
#6473 = EDGE_CURVE ( 'NONE', #4794, #6904, #12915, .T. ) ;
#6474 = EDGE_LOOP ( 'NONE', ( #468, #8610 ) ) ;
#6475 = CARTESIAN_POINT ( 'NONE',  ( -1.398371068895200908, -0.02596287309409977401, -0.07122367060404551087 ) ) ;
#6476 = DIRECTION ( 'NONE',  ( -0.000000000000000000, -0.000000000000000000, -1.000000000000000000 ) ) ;
#6477 = CARTESIAN_POINT ( 'NONE',  ( 0.2393297813660762996, -0.4881889763779528324, 0.06089400679746265199 ) ) ;
#6478 = EDGE_CURVE ( 'NONE', #10823, #6490, #1411, .T. ) ;
#6479 = FACE_OUTER_BOUND ( 'NONE', #12934, .T. ) ;
#6480 = CYLINDRICAL_SURFACE ( 'NONE', #4606, 0.03937007874015751446 ) ;
#6481 = EDGE_CURVE ( 'NONE', #880, #14915, #1909, .T. ) ;
#6482 = DIRECTION ( 'NONE',  ( 0.000000000000000000, 1.000000000000000000, 0.000000000000000000 ) ) ;
#6483 = CARTESIAN_POINT ( 'NONE',  ( 0.1062992125984796865, -0.09842519685039370636, -0.5870514566507987197 ) ) ;
#6484 = DIRECTION ( 'NONE',  ( 0.000000000000000000, 0.000000000000000000, -1.000000000000000000 ) ) ;
#6485 = CARTESIAN_POINT ( 'NONE',  ( -1.887622960209728307, -2.902805997487048373, -0.07702258022142625948 ) ) ;
#6486 = EDGE_LOOP ( 'NONE', ( #1054, #2961 ) ) ;
#6487 = LINE ( 'NONE', #8770, #1440 ) ;
#6488 = CARTESIAN_POINT ( 'NONE',  ( -0.004690417658706399866, 0.1529805375610462648, -0.008482181431098845953 ) ) ;
#6489 = ORIENTED_EDGE ( 'NONE', *, *, #3176, .F. ) ;
#6490 = VERTEX_POINT ( 'NONE', #13969 ) ;
#6491 = ORIENTED_EDGE ( 'NONE', *, *, #14094, .F. ) ;
#6492 = DIRECTION ( 'NONE',  ( 1.000000000000000000, -1.734723475976817507E-14, 0.000000000000000000 ) ) ;
#6493 = CARTESIAN_POINT ( 'NONE',  ( 0.2681506793018588741, -0.1023622047244094474, 0.03207310886168006359 ) ) ;
#6494 = DIRECTION ( 'NONE',  ( 0.5000000000000035527, 0.000000000000000000, -0.8660254037844365982 ) ) ;
#6495 = CARTESIAN_POINT ( 'NONE',  ( -0.5860051159906336515, -0.09448818897637796532, 0.1591122789105256508 ) ) ;
#6496 = EDGE_LOOP ( 'NONE', ( #14552, #9244, #5733, #5177 ) ) ;
#6497 = DIRECTION ( 'NONE',  ( -0.5000000000000004441, 0.000000000000000000, -0.8660254037844383745 ) ) ;
#6498 = FACE_OUTER_BOUND ( 'NONE', #1072, .T. ) ;
#6499 = CARTESIAN_POINT ( 'NONE',  ( -0.007502606504445189818, -0.1783918715466211447, 0.01493773385587683113 ) ) ;
#6500 = DIRECTION ( 'NONE',  ( -0.000000000000000000, -1.000000000000000000, -0.000000000000000000 ) ) ;
#6501 = DIRECTION ( 'NONE',  ( 1.000000000000000000, -0.000000000000000000, -0.000000000000000000 ) ) ;
#6502 = EDGE_LOOP ( 'NONE', ( #3321, #13382, #10226, #13720 ) ) ;
#6503 = ORIENTED_EDGE ( 'NONE', *, *, #12210, .T. ) ;
#6504 = DIRECTION ( 'NONE',  ( -0.000000000000000000, -1.000000000000000000, -0.000000000000000000 ) ) ;
#6505 = DIRECTION ( 'NONE',  ( -3.469446951953612927E-14, 0.000000000000000000, -1.000000000000000000 ) ) ;
#6506 = FACE_OUTER_BOUND ( 'NONE', #7578, .T. ) ;
#6507 = FACE_OUTER_BOUND ( 'NONE', #9574, .T. ) ;
#6508 = CARTESIAN_POINT ( 'NONE',  ( 0.000000000000000000, 0.3070866141732283561, 0.000000000000000000 ) ) ;
#6509 = EDGE_CURVE ( 'NONE', #2574, #7829, #6909, .T. ) ;
#6510 = DIRECTION ( 'NONE',  ( -0.4274092037376938102, 0.000000000000000000, -0.9040582794047684612 ) ) ;
#6511 = DIRECTION ( 'NONE',  ( 0.8660254037844383745, 0.000000000000000000, -0.5000000000000004441 ) ) ;
#6512 = FACE_OUTER_BOUND ( 'NONE', #1515, .T. ) ;
#6513 = CARTESIAN_POINT ( 'NONE',  ( -0.2642136714276788201, -0.4921259842519685179, 0.03889220652917903254 ) ) ;
#6514 = ADVANCED_FACE ( 'NONE', ( #15059 ), #8915, .T. ) ;
#6515 = LINE ( 'NONE', #4026, #9424 ) ;
#6516 = ORIENTED_EDGE ( 'NONE', *, *, #13927, .F. ) ;
#6517 = ORIENTED_EDGE ( 'NONE', *, *, #13276, .F. ) ;
#6518 = EDGE_LOOP ( 'NONE', ( #13574, #4209, #10763, #7001 ) ) ;
#6519 = VERTEX_POINT ( 'NONE', #4310 ) ;
#6520 = EDGE_CURVE ( 'NONE', #10948, #14791, #14925, .T. ) ;
#6521 = CYLINDRICAL_SURFACE ( 'NONE', #596, 0.01968503937007871907 ) ;
#6522 = CARTESIAN_POINT ( 'NONE',  ( -2.007604201720935677, -2.768319273907016154, 0.1776676917229350894 ) ) ;
#6523 = SHAPE_REPRESENTATION_RELATIONSHIP ( 'NONE' , 'NONE' ,  #6262, #15308 ) ;
#6524 = ADVANCED_FACE ( 'NONE', ( #3236, #5646 ), #12638, .F. ) ;
#6525 = CARTESIAN_POINT ( 'NONE',  ( 0.5412478373021326616, 0.000000000000000000, 0.2362233606508025163 ) ) ;
#6526 = CARTESIAN_POINT ( 'NONE',  ( -1.981870241362710061, -2.839422880978404784, -0.1645059300150371884 ) ) ;
#6527 = CARTESIAN_POINT ( 'NONE',  ( 0.000000000000000000, -0.4881889763779528324, -0.5870514566507987197 ) ) ;
#6528 = DIRECTION ( 'NONE',  ( 0.000000000000000000, 4.565061778886334044E-16, 1.000000000000000000 ) ) ;
#6529 = CARTESIAN_POINT ( 'NONE',  ( -1.915493804681331680, -2.830794960306212360, 0.1437166327912214048 ) ) ;
#6530 = EDGE_CURVE ( 'NONE', #2559, #11019, #5491, .T. ) ;
#6531 = CARTESIAN_POINT ( 'NONE',  ( -0.5595825771504281398, -0.4921259842519685179, 0.2048774586467239367 ) ) ;
#6532 = CARTESIAN_POINT ( 'NONE',  ( -0.1629063847838169987, -0.4921259842519685179, 0.2122517380126066888 ) ) ;
#6533 = ORIENTED_EDGE ( 'NONE', *, *, #4978, .T. ) ;
#6534 = VERTEX_POINT ( 'NONE', #13885 ) ;
#6535 = ORIENTED_EDGE ( 'NONE', *, *, #14776, .F. ) ;
#6536 = EDGE_LOOP ( 'NONE', ( #10760, #15280, #7585, #6242 ) ) ;
#6537 = ORIENTED_EDGE ( 'NONE', *, *, #9047, .T. ) ;
#6538 = FACE_OUTER_BOUND ( 'NONE', #8325, .T. ) ;
#6539 = FACE_OUTER_BOUND ( 'NONE', #4210, .T. ) ;
#6540 = DIRECTION ( 'NONE',  ( 0.000000000000000000, 0.000000000000000000, 1.000000000000000000 ) ) ;
#6541 = DIRECTION ( 'NONE',  ( 1.000000000000000000, 0.000000000000000000, 0.000000000000000000 ) ) ;
#6542 = DIRECTION ( 'NONE',  ( 0.000000000000000000, 0.000000000000000000, 1.000000000000000000 ) ) ;
#6543 = CARTESIAN_POINT ( 'NONE',  ( 1.224409448818897461, 4.044111181948214319E-16, -0.02559055118110236185 ) ) ;
#6544 = CARTESIAN_POINT ( 'NONE',  ( -0.4751993499419963074, 0.000000000000000000, 0.3506226965216301950 ) ) ;
#6545 = CARTESIAN_POINT ( 'NONE',  ( -0.5860051159906336515, -0.09448818897637796532, 0.1591122789105256785 ) ) ;
#6546 = CARTESIAN_POINT ( 'NONE',  ( 0.05905511811023622659, 1.043292445042268257, -0.5949473527966270270 ) ) ;
#6547 = ORIENTED_EDGE ( 'NONE', *, *, #5215, .T. ) ;
#6548 = DIRECTION ( 'NONE',  ( 0.000000000000000000, 0.000000000000000000, -1.000000000000000000 ) ) ;
#6549 = CARTESIAN_POINT ( 'NONE',  ( -0.2613315816341005848, -0.4881889763779528324, 0.03601011673560078341 ) ) ;
#6550 = EDGE_CURVE ( 'NONE', #12673, #14162, #664, .T. ) ;
#6551 = ORIENTED_EDGE ( 'NONE', *, *, #5215, .F. ) ;
#6552 = ORIENTED_EDGE ( 'NONE', *, *, #1543, .F. ) ;
#6553 = ADVANCED_FACE ( 'NONE', ( #8006 ), #3158, .T. ) ;
#6554 = EDGE_LOOP ( 'NONE', ( #11932, #2542, #15160, #2042 ) ) ;
#6555 = CIRCLE ( 'NONE', #8069, 0.007874015748031501158 ) ;
#6556 = VECTOR ( 'NONE', #5448, 39.37007874015748143 ) ;
#6557 = AXIS2_PLACEMENT_3D ( 'NONE', #12602, #11428, #705 ) ;
#6558 = LINE ( 'NONE', #11354, #14120 ) ;
#6559 = DIRECTION ( 'NONE',  ( 0.8660254037844254960, -0.000000000000000000, 0.5000000000000228706 ) ) ;
#6560 = LINE ( 'NONE', #11356, #202 ) ;
#6561 = DIRECTION ( 'NONE',  ( 0.4999999999999996114, 0.000000000000000000, 0.8660254037844389297 ) ) ;
#6562 = CARTESIAN_POINT ( 'NONE',  ( -0.05916619364927751951, -0.1856756262235988719, -0.05712045715993030459 ) ) ;
#6563 = EDGE_CURVE ( 'NONE', #5839, #13855, #7403, .T. ) ;
#6564 = VERTEX_POINT ( 'NONE', #5416 ) ;
#6565 = DIRECTION ( 'NONE',  ( 0.000000000000000000, 0.000000000000000000, 1.000000000000000000 ) ) ;
#6566 = CARTESIAN_POINT ( 'NONE',  ( 0.000000000000000000, 1.425196850393700920, 0.000000000000000000 ) ) ;
#6567 = AXIS2_PLACEMENT_3D ( 'NONE', #13929, #2086, #4687 ) ;
#6568 = CIRCLE ( 'NONE', #13587, 0.003937007874015750579 ) ;
#6569 = CARTESIAN_POINT ( 'NONE',  ( -0.007978440472143270498, -0.1611588996411620900, 0.01594766689393424530 ) ) ;
#6570 = DIRECTION ( 'NONE',  ( 0.000000000000000000, -0.000000000000000000, -1.000000000000000000 ) ) ;
#6571 = VECTOR ( 'NONE', #15450, 39.37007874015748143 ) ;
#6572 = DIRECTION ( 'NONE',  ( -0.4999999999999979461, 0.000000000000000000, -0.8660254037844398178 ) ) ;
#6573 = CIRCLE ( 'NONE', #8089, 0.5905511811023621549 ) ;
#6574 = ORIENTED_EDGE ( 'NONE', *, *, #7051, .F. ) ;
#6575 = ORIENTED_EDGE ( 'NONE', *, *, #13446, .F. ) ;
#6576 = VERTEX_POINT ( 'NONE', #659 ) ;
#6577 = CARTESIAN_POINT ( 'NONE',  ( -1.181102362204724310, 0.1240157480314959815, 0.02559055118110236185 ) ) ;
#6578 = AXIS2_PLACEMENT_3D ( 'NONE', #4756, #2482, #7322 ) ;
#6579 = AXIS2_PLACEMENT_3D ( 'NONE', #3495, #2384, #7166 ) ;
#6580 = VECTOR ( 'NONE', #7620, 39.37007874015748143 ) ;
#6581 = CARTESIAN_POINT ( 'NONE',  ( -0.05639125304298477775, 0.1674615591801703607, -0.03403793048618272005 ) ) ;
#6582 = CARTESIAN_POINT ( 'NONE',  ( -1.293236445124221312, 0.1355266887446167634, 0.05905511811023622659 ) ) ;
#6583 = AXIS2_PLACEMENT_3D ( 'NONE', #13435, #14836, #13669 ) ;
#6584 =( NAMED_UNIT ( * ) PLANE_ANGLE_UNIT ( ) SI_UNIT ( $, .RADIAN. ) );
#6585 = CARTESIAN_POINT ( 'NONE',  ( 0.000000000000000000, 2.440944881889763884, -0.5826771653543306728 ) ) ;
#6586 = CARTESIAN_POINT ( 'NONE',  ( 0.5433070866142283295, -0.4881889763779528324, 0.2409414509217496780 ) ) ;
#6587 = ORIENTED_EDGE ( 'NONE', *, *, #546, .F. ) ;
#6588 = CARTESIAN_POINT ( 'NONE',  ( -2.169366242005652534, -2.077173998931358234, -0.09331536252806053866 ) ) ;
#6589 = CARTESIAN_POINT ( 'NONE',  ( 0.1638199706403873079, -0.1023622047244094474, 0.2127791970528254417 ) ) ;
#6590 = CARTESIAN_POINT ( 'NONE',  ( 0.000000000000000000, 0.003937007874015749712, 0.000000000000000000 ) ) ;
#6591 = LINE ( 'NONE', #5430, #13176 ) ;
#6592 = CIRCLE ( 'NONE', #2603, 0.003937007874015721089 ) ;
#6593 = VERTEX_POINT ( 'NONE', #10441 ) ;
#6594 = EDGE_CURVE ( 'NONE', #9393, #9540, #11582, .T. ) ;
#6595 = AXIS2_PLACEMENT_3D ( 'NONE', #6962, #5840, #4695 ) ;
#6596 = ORIENTED_EDGE ( 'NONE', *, *, #12228, .F. ) ;
#6597 = CIRCLE ( 'NONE', #9880, 0.003937007874015737569 ) ;
#6598 = EDGE_CURVE ( 'NONE', #7333, #5666, #970, .T. ) ;
#6599 = ORIENTED_EDGE ( 'NONE', *, *, #10460, .T. ) ;
#6600 = AXIS2_PLACEMENT_3D ( 'NONE', #6044, #348, #11061 ) ;
#6601 = ADVANCED_FACE ( 'NONE', ( #1814 ), #2215, .T. ) ;
#6602 = DIRECTION ( 'NONE',  ( -0.000000000000000000, -0.000000000000000000, -1.000000000000000000 ) ) ;
#6603 = FACE_OUTER_BOUND ( 'NONE', #6836, .T. ) ;
#6604 = AXIS2_PLACEMENT_3D ( 'NONE', #11297, #11386, #10137 ) ;
#6605 = AXIS2_PLACEMENT_3D ( 'NONE', #12735, #4492, #15130 ) ;
#6606 = CYLINDRICAL_SURFACE ( 'NONE', #12464, 0.003937007874015759253 ) ;
#6607 = CLOSED_SHELL ( 'NONE', ( #9187, #11543, #8946 ) ) ;
#6608 = CARTESIAN_POINT ( 'NONE',  ( -1.988607233356104009, -2.761830767068704784, -0.1772894973384211703 ) ) ;
#6609 = CARTESIAN_POINT ( 'NONE',  ( -0.03346456692913318126, -0.4921259842519685179, 0.05796233017454786168 ) ) ;
#6610 = AXIS2_PLACEMENT_3D ( 'NONE', #4155, #2908, #7684 ) ;
#6611 = CARTESIAN_POINT ( 'NONE',  ( 0.06473829668901658063, 0.07239639532902293617, 0.04482148303915918508 ) ) ;
#6612 = CARTESIAN_POINT ( 'NONE',  ( -2.168820329264121494, -1.823085014281403682, -0.1033464566929124112 ) ) ;
#6613 = CARTESIAN_POINT ( 'NONE',  ( -2.080682670864669515, -2.105520006804255218, -0.09620997013695481437 ) ) ;
#6614 = ORIENTED_EDGE ( 'NONE', *, *, #13199, .T. ) ;
#6615 = ORIENTED_EDGE ( 'NONE', *, *, #1426, .F. ) ;
#6616 = EDGE_CURVE ( 'NONE', #5070, #12857, #3619, .T. ) ;
#6617 = CIRCLE ( 'NONE', #10396, 0.08858267716535432601 ) ;
#6618 = ORIENTED_EDGE ( 'NONE', *, *, #15256, .F. ) ;
#6619 = TOROIDAL_SURFACE ( 'NONE', #1644, 0.7007874015748031260, 0.007874015748031495954 ) ;
#6620 = ADVANCED_FACE ( 'NONE', ( #3701 ), #3579, .F. ) ;
#6621 = ORIENTED_EDGE ( 'NONE', *, *, #614, .T. ) ;
#6622 = CIRCLE ( 'NONE', #8144, 0.6692913385826770867 ) ;
#6623 = CARTESIAN_POINT ( 'NONE',  ( 7.232166136696967594E-17, 0.000000000000000000, 0.5905511811023621549 ) ) ;
#6624 = ADVANCED_FACE ( 'NONE', ( #14274 ), #5959, .F. ) ;
#6625 = CARTESIAN_POINT ( 'NONE',  ( -0.06604848736013260724, 1.346456692913385877, -0.5868460571724354313 ) ) ;
#6626 = CARTESIAN_POINT ( 'NONE',  ( -0.4319503555479016765, -0.2952755905511811330, 0.1766496122645288547 ) ) ;
#6627 = CARTESIAN_POINT ( 'NONE',  ( -2.010991777528384983, -2.758467574604075434, 0.1561691687464104861 ) ) ;
#6628 = DIRECTION ( 'NONE',  ( 0.000000000000000000, 0.000000000000000000, -1.000000000000000000 ) ) ;
#6629 = DIRECTION ( 'NONE',  ( -0.000000000000000000, 1.000000000000000000, 0.000000000000000000 ) ) ;
#6630 = FACE_OUTER_BOUND ( 'NONE', #12486, .T. ) ;
#6631 = CIRCLE ( 'NONE', #9156, 0.003937007874015758385 ) ;
#6632 = CARTESIAN_POINT ( 'NONE',  ( 0.05905511811023622659, 1.338582677165354395, -0.8267716535433070613 ) ) ;
#6633 = CIRCLE ( 'NONE', #3418, 0.1535433070866141780 ) ;
#6634 = SPHERICAL_SURFACE ( 'NONE', #393, 0.01968503937007873988 ) ;
#6635 = VECTOR ( 'NONE', #4089, 39.37007874015747433 ) ;
#6636 = ORIENTED_EDGE ( 'NONE', *, *, #2648, .F. ) ;
#6637 = DIRECTION ( 'NONE',  ( -0.000000000000000000, 0.000000000000000000, 1.000000000000000000 ) ) ;
#6638 = CARTESIAN_POINT ( 'NONE',  ( 0.5576140732134206024, -0.4881889763779528324, 0.2082870074805215910 ) ) ;
#6639 = CIRCLE ( 'NONE', #1907, 0.1653543307086614012 ) ;
#6640 = ORIENTED_EDGE ( 'NONE', *, *, #9503, .T. ) ;
#6641 = EDGE_LOOP ( 'NONE', ( #13801, #987, #1160, #1941 ) ) ;
#6642 = ADVANCED_FACE ( 'NONE', ( #13251 ), #4639, .T. ) ;
#6643 = ORIENTED_EDGE ( 'NONE', *, *, #5290, .F. ) ;
#6644 =( GEOMETRIC_REPRESENTATION_CONTEXT ( 3 ) GLOBAL_UNCERTAINTY_ASSIGNED_CONTEXT ( ( #14747 ) ) GLOBAL_UNIT_ASSIGNED_CONTEXT ( ( #9518, #14370, #9277 ) ) REPRESENTATION_CONTEXT ( 'NONE', 'WORKASPACE' ) );
#6645 = CARTESIAN_POINT ( 'NONE',  ( 0.000000000000000000, 0.000000000000000000, -0.6692913385826770867 ) ) ;
#6646 = EDGE_CURVE ( 'NONE', #12485, #1542, #13575, .T. ) ;
#6647 = AXIS2_PLACEMENT_3D ( 'NONE', #4790, #5015, #7370 ) ;
#6648 = DIRECTION ( 'NONE',  ( 0.000000000000000000, 0.000000000000000000, -1.000000000000000000 ) ) ;
#6649 = CARTESIAN_POINT ( 'NONE',  ( -0.1724006475077544953, -0.4921259842519685179, 0.1768186671464649640 ) ) ;
#6650 = DIRECTION ( 'NONE',  ( -0.4999999999999975575, 0.000000000000000000, 0.8660254037844399289 ) ) ;
#6651 = FACE_OUTER_BOUND ( 'NONE', #12926, .T. ) ;
#6652 = DIRECTION ( 'NONE',  ( 0.5000000000000004441, 1.502314598737158676E-14, -0.8660254037844383745 ) ) ;
#6653 = EDGE_LOOP ( 'NONE', ( #110, #10461, #8686 ) ) ;
#6654 = DIRECTION ( 'NONE',  ( 0.8660254037844387076, 0.000000000000000000, -0.4999999999999999445 ) ) ;
#6655 = EDGE_CURVE ( 'NONE', #9377, #10277, #1338, .T. ) ;
#6656 = CARTESIAN_POINT ( 'NONE',  ( 0.5894146648244296127, -0.09842519685039370636, 0.1610807828475372405 ) ) ;
#6657 = CIRCLE ( 'NONE', #12197, 0.04330708661417324162 ) ;
#6658 = CARTESIAN_POINT ( 'NONE',  ( -0.03005672326763337773, -0.1816858507396494349, 0.01806077797202005480 ) ) ;
#6659 = CARTESIAN_POINT ( 'NONE',  ( -0.1574803149606299191, -0.09448818897637796532, -0.5870514566507987197 ) ) ;
#6660 = VERTEX_POINT ( 'NONE', #14438 ) ;
#6661 = CIRCLE ( 'NONE', #6159, 0.003937007874015721089 ) ;
#6662 = ORIENTED_EDGE ( 'NONE', *, *, #10181, .F. ) ;
#6663 = AXIS2_PLACEMENT_3D ( 'NONE', #887, #1914, #12793 ) ;
#6664 = ORIENTED_EDGE ( 'NONE', *, *, #14396, .T. ) ;
#6665 = ORIENTED_EDGE ( 'NONE', *, *, #11434, .F. ) ;
#6666 = DIRECTION ( 'NONE',  ( 0.000000000000000000, 0.000000000000000000, 1.000000000000000000 ) ) ;
#6667 = CARTESIAN_POINT ( 'NONE',  ( -0.1022864650139100884, 0.05905511811023622659, -1.048351444896847144E-20 ) ) ;
#6668 = VECTOR ( 'NONE', #8511, 39.37007874015748143 ) ;
#6669 = CARTESIAN_POINT ( 'NONE',  ( -0.000000000000000000, -0.09842519685039370636, -0.5870514566507987197 ) ) ;
#6670 = CARTESIAN_POINT ( 'NONE',  ( 0.000000000000000000, 0.05905511811023622659, 0.000000000000000000 ) ) ;
#6671 = APPLICATION_PROTOCOL_DEFINITION ( 'draft international standard', 'automotive_design', 1998, #1104 ) ;
#6672 = CARTESIAN_POINT ( 'NONE',  ( -0.2681506793016945611, -0.1023622047244094474, 0.03207310886158502850 ) ) ;
#6673 = AXIS2_PLACEMENT_3D ( 'NONE', #9394, #3209, #3446 ) ;
#6674 = PLANE ( 'NONE',  #7606 ) ;
#6675 = EDGE_LOOP ( 'NONE', ( #3923, #7007, #12519, #5023, #6533, #14553, #13923 ) ) ;
#6676 = FACE_OUTER_BOUND ( 'NONE', #13656, .T. ) ;
#6677 = EDGE_CURVE ( 'NONE', #2728, #2681, #8583, .T. ) ;
#6678 = CARTESIAN_POINT ( 'NONE',  ( -1.568343923620152625, 0.1178486908565802016, -0.03937007874015747977 ) ) ;
#6679 = AXIS2_PLACEMENT_3D ( 'NONE', #261, #2813, #13319 ) ;
#6680 = CARTESIAN_POINT ( 'NONE',  ( 0.1181102362204724532, 2.637795275590551825, -0.03937007874015747977 ) ) ;
#6681 = CARTESIAN_POINT ( 'NONE',  ( -1.419615703680148000, -0.01226548409420230579, 0.08366141732283458032 ) ) ;
#6682 = ORIENTED_EDGE ( 'NONE', *, *, #6616, .F. ) ;
#6683 = AXIS2_PLACEMENT_3D ( 'NONE', #11406, #13824, #11247 ) ;
#6684 = ORIENTED_EDGE ( 'NONE', *, *, #13073, .T. ) ;
#6685 = VERTEX_POINT ( 'NONE', #2512 ) ;
#6686 = AXIS2_PLACEMENT_3D ( 'NONE', #1477, #7415, #10526 ) ;
#6687 = ORIENTED_EDGE ( 'NONE', *, *, #918, .T. ) ;
#6688 = DIRECTION ( 'NONE',  ( 0.000000000000000000, 0.000000000000000000, 1.000000000000000000 ) ) ;
#6689 = CARTESIAN_POINT ( 'NONE',  ( -2.003332662134895248, -2.780495179851753207, 0.1775193625598680269 ) ) ;
#6690 = B_SPLINE_CURVE_WITH_KNOTS ( 'NONE', 3,
 ( #6209, #14694, #3953, #13500, #10921, #2766, #8730, #11149, #9987, #12102 ),
 .UNSPECIFIED., .F., .F.,
 ( 4, 2, 2, 2, 4 ),
 ( 0.000000000000000000, 0.0002149660118259327313, 0.0004299320236518654626, 0.0006448980354777981939, 0.0008598640473037309252 ),
 .UNSPECIFIED. ) ;
#6691 = AXIS2_PLACEMENT_3D ( 'NONE', #3427, #102, #9138 ) ;
#6692 = CARTESIAN_POINT ( 'NONE',  ( 0.000000000000000000, 1.606299212598425674, 0.000000000000000000 ) ) ;
#6693 =( REPRESENTATION_RELATIONSHIP ('NONE','NONE', #8904, #11075 ) REPRESENTATION_RELATIONSHIP_WITH_TRANSFORMATION ( #12792 )SHAPE_REPRESENTATION_RELATIONSHIP( ) );
#6694 = CARTESIAN_POINT ( 'NONE',  ( -1.972648348582522360, -2.863648286116795116, -0.1334986992619453527 ) ) ;
#6695 = DIRECTION ( 'NONE',  ( -0.000000000000000000, -0.000000000000000000, -1.000000000000000000 ) ) ;
#6696 = VECTOR ( 'NONE', #11525, 39.37007874015748143 ) ;
#6697 = CYLINDRICAL_SURFACE ( 'NONE', #12905, 0.1476377952755906775 ) ;
#6698 = PLANE ( 'NONE',  #13328 ) ;
#6699 = DIRECTION ( 'NONE',  ( -0.000000000000000000, -0.000000000000000000, -1.000000000000000000 ) ) ;
#6700 = ORIENTED_EDGE ( 'NONE', *, *, #7283, .F. ) ;
#6701 = EDGE_CURVE ( 'NONE', #13962, #7115, #10677, .T. ) ;
#6702 = ORIENTED_EDGE ( 'NONE', *, *, #2467, .F. ) ;
#6703 = AXIS2_PLACEMENT_3D ( 'NONE', #13642, #14578, #2750 ) ;
#6704 = VERTEX_POINT ( 'NONE', #9432 ) ;
#6705 = ORIENTED_EDGE ( 'NONE', *, *, #10139, .T. ) ;
#6706 = AXIS2_PLACEMENT_3D ( 'NONE', #4976, #11078, #12207 ) ;
#6707 = CARTESIAN_POINT ( 'NONE',  ( 0.05905511811029055813, -0.09842519685039370636, 8.537024980208681893E-18 ) ) ;
#6708 = DIRECTION ( 'NONE',  ( -0.000000000000000000, 1.000000000000000000, -0.000000000000000000 ) ) ;
#6709 = DIRECTION ( 'NONE',  ( 0.000000000000000000, 1.000000000000000000, 0.000000000000000000 ) ) ;
#6710 = DIRECTION ( 'NONE',  ( 0.000000000000000000, 1.000000000000000000, 0.000000000000000000 ) ) ;
#6711 = DIRECTION ( 'NONE',  ( 0.000000000000000000, 1.000000000000000000, 0.000000000000000000 ) ) ;
#6712 = PLANE ( 'NONE',  #386 ) ;
#6713 = DIRECTION ( 'NONE',  ( 0.000000000000000000, 1.000000000000000000, 0.000000000000000000 ) ) ;
#6714 = CARTESIAN_POINT ( 'NONE',  ( -1.904013713778871963, -2.861285413342554040, -0.1538978722022966983 ) ) ;
#6715 = EDGE_CURVE ( 'NONE', #4524, #12161, #4330, .T. ) ;
#6716 = ORIENTED_EDGE ( 'NONE', *, *, #13995, .T. ) ;
#6717 = CARTESIAN_POINT ( 'NONE',  ( -1.437672431148612429, -0.06355280397547365123, -0.08366141732283455257 ) ) ;
#6718 = CARTESIAN_POINT ( 'NONE',  ( -0.09842519685028353060, -0.4921259842519685179, -0.2482618547482104143 ) ) ;
#6719 = DIRECTION ( 'NONE',  ( -1.000000000000000000, 0.000000000000000000, 0.000000000000000000 ) ) ;
#6720 = EDGE_LOOP ( 'NONE', ( #10294, #5732, #13543, #5552 ) ) ;
#6721 = EDGE_CURVE ( 'NONE', #12158, #731, #6819, .T. ) ;
#6722 = VERTEX_POINT ( 'NONE', #2446 ) ;
#6723 = PRODUCT_DEFINITION_CONTEXT ( 'detailed design', #11291, 'design' ) ;
#6724 = ORIENTED_EDGE ( 'NONE', *, *, #13680, .T. ) ;
#6725 = CARTESIAN_POINT ( 'NONE',  ( 0.1023622047244638067, -0.4921259842519685179, -0.2482618547481154347 ) ) ;
#6726 = EDGE_CURVE ( 'NONE', #12058, #646, #12013, .T. ) ;
#6727 = FACE_OUTER_BOUND ( 'NONE', #12586, .T. ) ;
#6728 = CARTESIAN_POINT ( 'NONE',  ( -0.4854723491485721798, 1.043263280880422528, 0.3484785681409913738 ) ) ;
#6729 = DIRECTION ( 'NONE',  ( 0.000000000000000000, 0.000000000000000000, 1.000000000000000000 ) ) ;
#6730 = CARTESIAN_POINT ( 'NONE',  ( -0.3589087851413753083, -0.2952755905511811330, 0.1299329768165586318 ) ) ;
#6731 = CARTESIAN_POINT ( 'NONE',  ( 0.1629063847838169432, -0.4881889763779528324, 0.2122517380126066888 ) ) ;
#6732 = ADVANCED_FACE ( 'NONE', ( #5791 ), #4722, .F. ) ;
#6733 = VERTEX_POINT ( 'NONE', #6100 ) ;
#6734 = CARTESIAN_POINT ( 'NONE',  ( 0.7455328141524921737, 1.043307086614173151, 0.3622425942646917418 ) ) ;
#6735 = DIRECTION ( 'NONE',  ( 0.000000000000000000, -1.000000000000000000, 0.000000000000000000 ) ) ;
#6736 = DIRECTION ( 'NONE',  ( -0.000000000000000000, 0.000000000000000000, 1.000000000000000000 ) ) ;
#6737 = DIRECTION ( 'NONE',  ( -0.5005078764080090892, -0.7027276007401488389, 0.5056340423780217863 ) ) ;
#6738 = EDGE_LOOP ( 'NONE', ( #15047, #5947, #12904, #3663 ) ) ;
#6739 = EDGE_CURVE ( 'NONE', #1672, #9404, #582, .T. ) ;
#6740 = CARTESIAN_POINT ( 'NONE',  ( 0.000000000000000000, 2.161417322834645827, 0.000000000000000000 ) ) ;
#6741 = ORIENTED_EDGE ( 'NONE', *, *, #8268, .T. ) ;
#6742 = DIMENSIONAL_EXPONENTS ( 1.000000000000000000, 0.000000000000000000, 0.000000000000000000, 0.000000000000000000, 0.000000000000000000, 0.000000000000000000, 0.000000000000000000 ) ;
#6743 = ORIENTED_EDGE ( 'NONE', *, *, #6814, .T. ) ;
#6744 = VERTEX_POINT ( 'NONE', #9336 ) ;
#6745 = DIRECTION ( 'NONE',  ( 0.000000000000000000, 0.000000000000000000, 1.000000000000000000 ) ) ;
#6746 = DIRECTION ( 'NONE',  ( 0.000000000000000000, 0.000000000000000000, -1.000000000000000000 ) ) ;
#6747 = CARTESIAN_POINT ( 'NONE',  ( -0.01899774626693294735, 0.1736125314593147118, -0.03244910060854599987 ) ) ;
#6748 = DIRECTION ( 'NONE',  ( -0.8660254037844347108, 0.000000000000000000, -0.5000000000000069944 ) ) ;
#6749 = ITEM_DEFINED_TRANSFORMATION ( 'NONE', 'NONE', #14877,  #11481 ) ;
#6750 = FACE_BOUND ( 'NONE', #273, .T. ) ;
#6751 = LINE ( 'NONE', #14048, #9886 ) ;
#6752 = ORIENTED_EDGE ( 'NONE', *, *, #9270, .F. ) ;
#6753 = CARTESIAN_POINT ( 'NONE',  ( -0.1213717603336464113, 2.440944881889763884, 0.04263160285333146560 ) ) ;
#6754 = CARTESIAN_POINT ( 'NONE',  ( 1.224409448818897461, 4.044111181948214319E-16, 0.02952755905511811330 ) ) ;
#6755 = CARTESIAN_POINT ( 'NONE',  ( -0.1552072824047652788, -0.003937007874015747977, -0.5909884645248143498 ) ) ;
#6756 = ADVANCED_FACE ( 'NONE', ( #14114 ), #3393, .T. ) ;
#6757 = VERTEX_POINT ( 'NONE', #7057 ) ;
#6758 = CARTESIAN_POINT ( 'NONE',  ( -1.431036756819010769, -0.02829858486107881405, -0.1033464566929133133 ) ) ;
#6759 = ORIENTED_EDGE ( 'NONE', *, *, #10390, .T. ) ;
#6760 = EDGE_CURVE ( 'NONE', #5345, #1627, #7359, .T. ) ;
#6761 = VERTEX_POINT ( 'NONE', #2581 ) ;
#6762 = B_SPLINE_CURVE_WITH_KNOTS ( 'NONE', 3,
 ( #3251, #9280, #3317, #14139 ),
 .UNSPECIFIED., .F., .F.,
 ( 4, 4 ),
 ( 0.000000000000000000, 2.119993237936496015E-05 ),
 .UNSPECIFIED. ) ;
#6763 = EDGE_CURVE ( 'NONE', #14569, #5052, #2076, .T. ) ;
#6764 = DIRECTION ( 'NONE',  ( 0.4999999999999971134, 0.000000000000000000, 0.8660254037844402619 ) ) ;
#6765 = DIRECTION ( 'NONE',  ( 0.000000000000000000, -1.000000000000000000, 0.000000000000000000 ) ) ;
#6766 = PRODUCT_DEFINITION_SHAPE ( 'NONE', 'NONE',  #15482 ) ;
#6767 = DIRECTION ( 'NONE',  ( 0.8660254037844385966, -0.000000000000000000, 0.5000000000000001110 ) ) ;
#6768 = DIRECTION ( 'NONE',  ( 0.5000000000000004441, 0.000000000000000000, -0.8660254037844383745 ) ) ;
#6769 = FACE_OUTER_BOUND ( 'NONE', #5238, .T. ) ;
#6770 = CARTESIAN_POINT ( 'NONE',  ( 0.05905511811023622659, 1.338582677165354395, -0.8267716535433070613 ) ) ;
#6771 = CARTESIAN_POINT ( 'NONE',  ( -2.087354244661867142, -1.726823559470685332, -0.1037499983681600124 ) ) ;
#6772 = VERTEX_POINT ( 'NONE', #8927 ) ;
#6773 = ORIENTED_EDGE ( 'NONE', *, *, #1933, .F. ) ;
#6774 = VERTEX_POINT ( 'NONE', #13702 ) ;
#6775 = VERTEX_POINT ( 'NONE', #188 ) ;
#6776 = EDGE_CURVE ( 'NONE', #11239, #10074, #3301, .T. ) ;
#6777 =( REPRESENTATION_RELATIONSHIP ('NONE','NONE', #8904, #7785 ) REPRESENTATION_RELATIONSHIP_WITH_TRANSFORMATION ( #8480 )SHAPE_REPRESENTATION_RELATIONSHIP( ) );
#6778 = CARTESIAN_POINT ( 'NONE',  ( -1.588286453767307593, 0.1240441066498496892, -0.03937007874189642903 ) ) ;
#6779 = CARTESIAN_POINT ( 'NONE',  ( 0.000000000000000000, -0.09842519685039370636, 0.000000000000000000 ) ) ;
#6780 = CARTESIAN_POINT ( 'NONE',  ( 0.000000000000000000, 1.370078740157480546, 0.000000000000000000 ) ) ;
#6781 = CARTESIAN_POINT ( 'NONE',  ( 4.821444091131311524E-18, 0.06496062992125986590, 0.03937007874015747977 ) ) ;
#6782 = FACE_OUTER_BOUND ( 'NONE', #484, .T. ) ;
#6783 = CARTESIAN_POINT ( 'NONE',  ( 0.000000000000000000, 1.417322834645669438, 0.000000000000000000 ) ) ;
#6784 = CARTESIAN_POINT ( 'NONE',  ( 0.000000000000000000, 0.000000000000000000, 0.000000000000000000 ) ) ;
#6785 = CARTESIAN_POINT ( 'NONE',  ( -0.09842519685028353060, -0.4881889763779528324, -0.2482618547482104143 ) ) ;
#6786 = ORIENTED_EDGE ( 'NONE', *, *, #9898, .T. ) ;
#6787 = CARTESIAN_POINT ( 'NONE',  ( -0.5860051159906336515, -0.09448818897637796532, 0.1591122789105256785 ) ) ;
#6788 = LINE ( 'NONE', #7691, #14913 ) ;
#6789 = EDGE_LOOP ( 'NONE', ( #3568, #12354, #9748, #8493 ) ) ;
#6790 = ORIENTED_EDGE ( 'NONE', *, *, #12774, .T. ) ;
#6791 = ADVANCED_FACE ( 'NONE', ( #15028 ), #4133, .F. ) ;
#6792 = ORIENTED_EDGE ( 'NONE', *, *, #9226, .T. ) ;
#6793 = ADVANCED_FACE ( 'NONE', ( #13841 ), #13339, .T. ) ;
#6794 = DIRECTION ( 'NONE',  ( 0.000000000000000000, -0.000000000000000000, -1.000000000000000000 ) ) ;
#6795 = ADVANCED_FACE ( 'NONE', ( #259 ), #12095, .F. ) ;
#6796 = DIRECTION ( 'NONE',  ( 0.000000000000000000, 1.000000000000000000, 0.000000000000000000 ) ) ;
#6797 = CARTESIAN_POINT ( 'NONE',  ( -1.978180062195354694, -2.794907819778010616, -0.1760901428592002160 ) ) ;
#6798 = DIRECTION ( 'NONE',  ( 0.000000000000000000, -1.000000000000000000, 0.000000000000000000 ) ) ;
#6799 = DIRECTION ( 'NONE',  ( -0.8660254037844385966, 0.000000000000000000, 0.5000000000000000000 ) ) ;
#6800 = CARTESIAN_POINT ( 'NONE',  ( -1.431036756819011213, -0.02829858486107871343, 0.08366141732283458032 ) ) ;
#6801 = ORIENTED_EDGE ( 'NONE', *, *, #3396, .F. ) ;
#6802 = CARTESIAN_POINT ( 'NONE',  ( 0.5445274672588121812, 1.043263280880422528, 0.2461921031270739857 ) ) ;
#6803 = FACE_BOUND ( 'NONE', #7886, .T. ) ;
#6804 = CARTESIAN_POINT ( 'NONE',  ( -0.1062992125983148878, -0.09448818897637796532, -0.5870514566507987197 ) ) ;
#6805 = DIRECTION ( 'NONE',  ( 0.000000000000000000, 0.000000000000000000, 1.000000000000000000 ) ) ;
#6806 = ORIENTED_EDGE ( 'NONE', *, *, #6432, .T. ) ;
#6807 = DIRECTION ( 'NONE',  ( 0.000000000000000000, 0.000000000000000000, 1.000000000000000000 ) ) ;
#6808 = EDGE_LOOP ( 'NONE', ( #6724, #2, #13442, #2589 ) ) ;
#6809 = VERTEX_POINT ( 'NONE', #1430 ) ;
#6810 = ADVANCED_FACE ( 'NONE', ( #6539 ), #7564, .T. ) ;
#6811 = ORIENTED_EDGE ( 'NONE', *, *, #4003, .T. ) ;
#6812 = DIRECTION ( 'NONE',  ( -0.4999999999999983347, -1.560416818047080642E-14, -0.8660254037844395958 ) ) ;
#6813 = CARTESIAN_POINT ( 'NONE',  ( -0.01449560339480800153, 0.1719786949496021622, 3.288862647277781903E-16 ) ) ;
#6814 = EDGE_CURVE ( 'NONE', #2689, #13551, #8828, .T. ) ;
#6815 = CARTESIAN_POINT ( 'NONE',  ( -0.008695292838831351900, 0.1754324108224426804, -0.01747077667449336777 ) ) ;
#6816 = CARTESIAN_POINT ( 'NONE',  ( 0.6864776960422569463, 1.190944881889763884, 0.4645290592786023298 ) ) ;
#6817 = ADVANCED_FACE ( 'NONE', ( #14960 ), #13607, .T. ) ;
#6818 = CARTESIAN_POINT ( 'NONE',  ( 1.305118110236220152, 4.044111181948214319E-16, 0.02559055118110236185 ) ) ;
#6819 = CIRCLE ( 'NONE', #7086, 0.6614173228346456046 ) ;
#6820 = CIRCLE ( 'NONE', #2066, 0.003937007874015749712 ) ;
#6821 = DIRECTION ( 'NONE',  ( -0.5000000000000001110, 0.000000000000000000, 0.8660254037844385966 ) ) ;
#6822 = ORIENTED_EDGE ( 'NONE', *, *, #2835, .F. ) ;
#6823 = LINE ( 'NONE', #8256, #8414 ) ;
#6824 = AXIS2_PLACEMENT_3D ( 'NONE', #5211, #10007, #12901 ) ;
#6825 = VECTOR ( 'NONE', #2659, 39.37007874015748143 ) ;
#6826 = DIRECTION ( 'NONE',  ( -0.000000000000000000, 1.000000000000000000, -0.000000000000000000 ) ) ;
#6827 = FILL_AREA_STYLE ('',( #10453 ) ) ;
#6828 = LINE ( 'NONE', #12877, #8179 ) ;
#6829 = ORIENTED_EDGE ( 'NONE', *, *, #1673, .F. ) ;
#6830 = EDGE_LOOP ( 'NONE', ( #7073, #3112, #8072, #13698 ) ) ;
#6831 = DIRECTION ( 'NONE',  ( -0.4999999999999919509, 0.000000000000000000, 0.8660254037844432595 ) ) ;
#6833 = ORIENTED_EDGE ( 'NONE', *, *, #8780, .T. ) ;
#6832 = AXIS2_PLACEMENT_3D ( 'NONE', #12119, #1389, #13447 ) ;
#6834 = AXIS2_PLACEMENT_3D ( 'NONE', #2385, #10465, #9366 ) ;
#6835 = EDGE_CURVE ( 'NONE', #5898, #6393, #7805, .T. ) ;
#6836 = EDGE_LOOP ( 'NONE', ( #4227, #6264, #6945, #7110 ) ) ;
#6837 = CIRCLE ( 'NONE', #13341, 0.03937007874015761161 ) ;
#6838 = ORIENTED_EDGE ( 'NONE', *, *, #145, .F. ) ;
#6839 = VECTOR ( 'NONE', #5088, 39.37007874015748143 ) ;
#6840 = EDGE_CURVE ( 'NONE', #11443, #14199, #9001, .T. ) ;
#6841 = DIRECTION ( 'NONE',  ( -1.000000000000000000, 0.000000000000000000, 0.000000000000000000 ) ) ;
#6842 = CARTESIAN_POINT ( 'NONE',  ( -0.03886060139087894189, 0.07874015748031495954, -0.08219815605944147396 ) ) ;
#6843 = LENGTH_MEASURE_WITH_UNIT ( LENGTH_MEASURE( 0.02539999999999999897 ), #3497 );
#6844 = ADVANCED_FACE ( 'NONE', ( #7661 ), #5286, .F. ) ;
#6845 = DIRECTION ( 'NONE',  ( 0.000000000000000000, 1.000000000000000000, 0.000000000000000000 ) ) ;
#6846 = FACE_OUTER_BOUND ( 'NONE', #7605, .T. ) ;
#6847 = VECTOR ( 'NONE', #14798, 39.37007874015748143 ) ;
#6848 = VECTOR ( 'NONE', #15164, 39.37007874015748143 ) ;
#6849 = COLOUR_RGB ( '',0.7921568627450980005, 0.8196078431372548767, 0.9333333333333333481 ) ;
#6850 = EDGE_CURVE ( 'NONE', #14540, #1004, #5903, .T. ) ;
#6851 = LINE ( 'NONE', #6770, #839 ) ;
#6852 = PLANE ( 'NONE',  #2902 ) ;
#6853 = TOROIDAL_SURFACE ( 'NONE', #3614, 0.04330708661417328326, 0.003937007874015747977 ) ;
#6854 = AXIS2_PLACEMENT_3D ( 'NONE', #11471, #4176, #11231 ) ;
#6855 = VERTEX_POINT ( 'NONE', #6625 ) ;
#6856 = PRODUCT_DEFINITION_FORMATION_WITH_SPECIFIED_SOURCE ( 'ANY', '', #5029, .NOT_KNOWN. ) ;
#6857 = VERTEX_POINT ( 'NONE', #12681 ) ;
#6858 = VERTEX_POINT ( 'NONE', #4278 ) ;
#6859 = ORIENTED_EDGE ( 'NONE', *, *, #7400, .F. ) ;
#6860 = CIRCLE ( 'NONE', #10370, 0.05905511811023625435 ) ;
#6861 = AXIS2_PLACEMENT_3D ( 'NONE', #11066, #12195, #11003 ) ;
#6862 = AXIS2_PLACEMENT_3D ( 'NONE', #9554, #6077, #7269 ) ;
#6863 = CARTESIAN_POINT ( 'NONE',  ( 0.5649606299212333038, -0.1023622047244094474, 0.2034364137499354852 ) ) ;
#6864 = DIRECTION ( 'NONE',  ( -0.000000000000000000, 0.000000000000000000, 1.000000000000000000 ) ) ;
#6865 = DIRECTION ( 'NONE',  ( 4.292327424963333000E-16, 1.000000000000000000, 2.478176394252540219E-16 ) ) ;
#6866 = AXIS2_PLACEMENT_3D ( 'NONE', #15044, #8779, #13548 ) ;
#6867 = CARTESIAN_POINT ( 'NONE',  ( -0.07278938515218676131, 0.1649651754370965173, 0.05936614484719628104 ) ) ;
#6868 = CARTESIAN_POINT ( 'NONE',  ( -0.5413385826771385245, -0.09448818897637796532, 0.2443509997554989266 ) ) ;
#6869 = CARTESIAN_POINT ( 'NONE',  ( 0.3964138223131414840, -0.2952755905511811330, 0.1515865201236449578 ) ) ;
#6870 = DIRECTION ( 'NONE',  ( -0.000000000000000000, -0.000000000000000000, -1.000000000000000000 ) ) ;
#6871 = FACE_OUTER_BOUND ( 'NONE', #5750, .T. ) ;
#6872 = CARTESIAN_POINT ( 'NONE',  ( -1.904866376297139841, -2.858959339525115162, -0.1270709863631420411 ) ) ;
#6873 = VERTEX_POINT ( 'NONE', #3116 ) ;
#6874 = DIRECTION ( 'NONE',  ( -0.4999999999999981681, 0.000000000000000000, -0.8660254037844397068 ) ) ;
#6875 = EDGE_CURVE ( 'NONE', #15288, #11324, #14088, .T. ) ;
#6876 = DIRECTION ( 'NONE',  ( 1.000000000000000000, 0.000000000000000000, -0.000000000000000000 ) ) ;
#6877 = VECTOR ( 'NONE', #3515, 39.37007874015748143 ) ;
#6878 = VECTOR ( 'NONE', #10755, 39.37007874015748143 ) ;
#6879 = TOROIDAL_SURFACE ( 'NONE', #146, 0.04330708661417326938, 0.003937007874015747977 ) ;
#6880 = ORIENTED_EDGE ( 'NONE', *, *, #1468, .T. ) ;
#6881 = VERTEX_POINT ( 'NONE', #15422 ) ;
#6882 = AXIS2_PLACEMENT_3D ( 'NONE', #11336, #7810, #10176 ) ;
#6883 = ORIENTED_EDGE ( 'NONE', *, *, #6073, .T. ) ;
#6884 = CARTESIAN_POINT ( 'NONE',  ( -0.09061599198715356018, 0.07874015748031495954, -0.007444810018878696839 ) ) ;
#6885 = TOROIDAL_SURFACE ( 'NONE', #405, 0.05905511811023621271, 0.01968503937007873988 ) ;
#6886 = CIRCLE ( 'NONE', #11392, 0.01968503937007875029 ) ;
#6887 = AXIS2_PLACEMENT_3D ( 'NONE', #11467, #1910, #4246 ) ;
#6888 = DIRECTION ( 'NONE',  ( -0.000000000000000000, -1.000000000000000000, -0.000000000000000000 ) ) ;
#6889 = CARTESIAN_POINT ( 'NONE',  ( -1.941383621697627682, -2.904153198872124975, -0.1189196622982612861 ) ) ;
#6890 = DIRECTION ( 'NONE',  ( 0.000000000000000000, -1.000000000000000000, 0.000000000000000000 ) ) ;
#6891 = DIRECTION ( 'NONE',  ( 0.8660254037844398178, -0.000000000000000000, -0.4999999999999979461 ) ) ;
#6892 = CIRCLE ( 'NONE', #11657, 0.03937007874015751446 ) ;
#6893 = CARTESIAN_POINT ( 'NONE',  ( 0.05905511811023622659, 1.043307086614173373, -0.5955041639236610118 ) ) ;
#6894 = EDGE_LOOP ( 'NONE', ( #10610, #11396, #8237, #3401 ) ) ;
#6895 = DIRECTION ( 'NONE',  ( -4.336808689942014285E-16, 0.000000000000000000, 1.000000000000000000 ) ) ;
#6896 = DIRECTION ( 'NONE',  ( 0.000000000000000000, 0.000000000000000000, -1.000000000000000000 ) ) ;
#6897 = CARTESIAN_POINT ( 'NONE',  ( -0.03749734052841491999, 0.1488898142811245495, 0.04795046931071418606 ) ) ;
#6898 = CARTESIAN_POINT ( 'NONE',  ( 0.4769054117961250561, -0.4921259842519685179, 0.3480785096661500599 ) ) ;
#6899 = VERTEX_POINT ( 'NONE', #2250 ) ;
#6900 = DIRECTION ( 'NONE',  ( -0.4999999999999981681, 0.000000000000000000, -0.8660254037844397068 ) ) ;
#6901 = CIRCLE ( 'NONE', #10909, 0.6692913385826770867 ) ;
#6902 = CIRCLE ( 'NONE', #2400, 0.5511811023622046335 ) ;
#6903 = CIRCLE ( 'NONE', #12880, 0.003937007874015758385 ) ;
#6904 = VERTEX_POINT ( 'NONE', #8128 ) ;
#6905 = ADVANCED_FACE ( 'NONE', ( #12911 ), #11330, .F. ) ;
#6906 = ORIENTED_EDGE ( 'NONE', *, *, #14219, .T. ) ;
#6907 = PRODUCT_DEFINITION_SHAPE ( 'NONE', 'NONE',  #15485 ) ;
#6908 = ORIENTED_EDGE ( 'NONE', *, *, #9584, .T. ) ;
#6909 = LINE ( 'NONE', #10280, #4901 ) ;
#6910 = DIRECTION ( 'NONE',  ( 0.000000000000000000, -1.000000000000000000, 0.000000000000000000 ) ) ;
#6911 = CARTESIAN_POINT ( 'NONE',  ( 0.5629921259843070347, -0.4921259842519685179, 0.2068459625837795746 ) ) ;
#6912 = FACE_OUTER_BOUND ( 'NONE', #8640, .T. ) ;
#6913 = FACE_OUTER_BOUND ( 'NONE', #6392, .T. ) ;
#6914 = VECTOR ( 'NONE', #8736, 39.37007874015748854 ) ;
#6915 = DIRECTION ( 'NONE',  ( 0.000000000000000000, -1.000000000000000000, -0.000000000000000000 ) ) ;
#6916 = ORIENTED_EDGE ( 'NONE', *, *, #14337, .T. ) ;
#6917 = EDGE_CURVE ( 'NONE', #12818, #9404, #1574, .T. ) ;
#6918 = CARTESIAN_POINT ( 'NONE',  ( 0.09842519685044820443, -0.4881889763779528324, -0.5909884645248143498 ) ) ;
#6919 = AXIS2_PLACEMENT_3D ( 'NONE', #8956, #1665, #14985 ) ;
#6920 = LINE ( 'NONE', #9516, #4701 ) ;
#6921 = EDGE_CURVE ( 'NONE', #11634, #13283, #11082, .T. ) ;
#6922 = CIRCLE ( 'NONE', #14439, 0.1279527559055117780 ) ;
#6923 = ORIENTED_EDGE ( 'NONE', *, *, #8733, .F. ) ;
#6924 = ORIENTED_EDGE ( 'NONE', *, *, #11278, .F. ) ;
#6925 = EDGE_CURVE ( 'NONE', #5035, #7635, #15182, .T. ) ;
#6926 = DIRECTION ( 'NONE',  ( 0.000000000000000000, 1.000000000000000000, 0.000000000000000000 ) ) ;
#6927 = ORIENTED_EDGE ( 'NONE', *, *, #308, .T. ) ;
#6928 = ORIENTED_EDGE ( 'NONE', *, *, #6178, .F. ) ;
#6929 = ORIENTED_EDGE ( 'NONE', *, *, #10953, .T. ) ;
#6930 = CARTESIAN_POINT ( 'NONE',  ( 0.000000000000000000, 0.07480314960629921850, 0.000000000000000000 ) ) ;
#6931 = AXIS2_PLACEMENT_3D ( 'NONE', #11670, #10490, #15339 ) ;
#6932 = CARTESIAN_POINT ( 'NONE',  ( 0.05114323250695499562, 0.000000000000000000, -0.08858267716535433989 ) ) ;
#6933 = CARTESIAN_POINT ( 'NONE',  ( -1.898417150026649125, -2.948016320718355399, -0.02360795789488797508 ) ) ;
#6934 = AXIS2_PLACEMENT_3D ( 'NONE', #4007, #12309, #2585 ) ;
#6935 = DIRECTION ( 'NONE',  ( 0.8660254037844368202, 0.000000000000000000, -0.5000000000000032196 ) ) ;
#6936 = CARTESIAN_POINT ( 'NONE',  ( 0.000000000000000000, 0.07480314960629921850, 0.000000000000000000 ) ) ;
#6937 = ADVANCED_FACE ( 'NONE', ( #930 ), #6363, .T. ) ;
#6938 = CARTESIAN_POINT ( 'NONE',  ( 0.1552072824047652233, -0.09842519685039370636, -0.5870514566507987197 ) ) ;
#6939 = DIRECTION ( 'NONE',  ( -0.000000000000000000, -0.000000000000000000, -1.000000000000000000 ) ) ;
#6940 = DIRECTION ( 'NONE',  ( -0.000000000000000000, -1.000000000000000000, -0.000000000000000000 ) ) ;
#6941 = TOROIDAL_SURFACE ( 'NONE', #11702, 0.1535433070866141780, 0.003937007874015747977 ) ;
#6942 = EDGE_CURVE ( 'NONE', #14238, #14453, #3833, .T. ) ;
#6943 = DIRECTION ( 'NONE',  ( -0.4999999999999979461, -0.000000000000000000, -0.8660254037844398178 ) ) ;
#6944 = CIRCLE ( 'NONE', #209, 0.007874015748031449116 ) ;
#6945 = ORIENTED_EDGE ( 'NONE', *, *, #10743, .T. ) ;
#6946 = EDGE_CURVE ( 'NONE', #13356, #6947, #5071, .T. ) ;
#6947 = VERTEX_POINT ( 'NONE', #8279 ) ;
#6948 = VERTEX_POINT ( 'NONE', #9232 ) ;
#6949 = ORIENTED_EDGE ( 'NONE', *, *, #14681, .F. ) ;
#6950 = VECTOR ( 'NONE', #2452, 39.37007874015748143 ) ;
#6951 = ADVANCED_FACE ( 'NONE', ( #5605 ), #13094, .T. ) ;
#6952 = CARTESIAN_POINT ( 'NONE',  ( 0.5379290338433416752, -0.1023622047244094474, 0.2423824958184916112 ) ) ;
#6953 = FACE_OUTER_BOUND ( 'NONE', #11888, .T. ) ;
#6954 = CARTESIAN_POINT ( 'NONE',  ( -0.5576140732134202693, -0.4881889763779528324, 0.2082870074805209248 ) ) ;
#6955 = CIRCLE ( 'NONE', #7958, 0.05905511811023625435 ) ;
#6956 = CARTESIAN_POINT ( 'NONE',  ( -0.04751022371102618658, 0.1688405673728185230, 0.05319490010182049977 ) ) ;
#6957 = DIRECTION ( 'NONE',  ( -1.000000000000000000, 0.000000000000000000, -0.000000000000000000 ) ) ;
#6958 = CARTESIAN_POINT ( 'NONE',  ( 0.3117681530218320840, -0.2952755905511811330, 0.2981971199768684855 ) ) ;
#6959 = CARTESIAN_POINT ( 'NONE',  ( -1.181102362204724310, 0.000000000000000000, -0.02559055118110236185 ) ) ;
#6960 = ORIENTED_EDGE ( 'NONE', *, *, #4615, .F. ) ;
#6961 = DIRECTION ( 'NONE',  ( 0.000000000000000000, -1.000000000000000000, -0.000000000000000000 ) ) ;
#6962 = CARTESIAN_POINT ( 'NONE',  ( 0.000000000000000000, 1.645669291338583085, 0.000000000000000000 ) ) ;
#6963 = CARTESIAN_POINT ( 'NONE',  ( 0.000000000000000000, -0.4881889763779528324, 0.000000000000000000 ) ) ;
#6964 = CIRCLE ( 'NONE', #5698, 0.003937007874015758385 ) ;
#6965 = ORIENTED_EDGE ( 'NONE', *, *, #11441, .F. ) ;
#6966 = EDGE_LOOP ( 'NONE', ( #3918, #12180, #6965 ) ) ;
#6967 = ADVANCED_FACE ( 'NONE', ( #9473 ), #15094, .T. ) ;
#6968 = CIRCLE ( 'NONE', #13727, 0.003937007874015758385 ) ;
#6969 = ORIENTED_EDGE ( 'NONE', *, *, #2241, .F. ) ;
#6970 = ADVANCED_FACE ( 'NONE', ( #9387 ), #14167, .F. ) ;
#6971 = CARTESIAN_POINT ( 'NONE',  ( -0.1734555655881918346, -0.1023622047244094474, 0.1689446513984334541 ) ) ;
#6972 = EDGE_CURVE ( 'NONE', #14775, #6434, #7581, .T. ) ;
#6973 = CARTESIAN_POINT ( 'NONE',  ( 0.2681506793018588186, -0.4921259842519685179, 0.03207310886168001501 ) ) ;
#6974 = CARTESIAN_POINT ( 'NONE',  ( -1.970940144590390908, -2.817289869702642946, -0.1717442269998073201 ) ) ;
#6975 = CARTESIAN_POINT ( 'NONE',  ( 1.928577636452524610E-17, 0.007874015748031480341, 0.1574803149606299191 ) ) ;
#6976 = CARTESIAN_POINT ( 'NONE',  ( -1.185322244937984104, 0.3350014259194302180, -0.05695314934227149739 ) ) ;
#6977 = EDGE_LOOP ( 'NONE', ( #15307, #1633 ) ) ;
#6978 = CARTESIAN_POINT ( 'NONE',  ( -2.182693454834259139, -1.630005269948474389, 0.08366141732283424726 ) ) ;
#6979 =( BOUNDED_SURFACE ( )  B_SPLINE_SURFACE ( 3, 2, ( 
 ( #11272, #2977, #14884 ),
 ( #11106, #399, #7672 ),
 ( #544, #3996, #6243 ),
 ( #8701, #485, #13783 ),
 ( #8842, #7815, #9960 ),
 ( #5387, #2892, #13621 ) ),
 .UNSPECIFIED., .F., .F., .T. ) 
 B_SPLINE_SURFACE_WITH_KNOTS ( ( 4, 2, 4 ),
 ( 3, 3 ),
 ( 0.000000000000000000, 0.01443577820670504351, 0.02887155641341008702 ),
 ( 0.000000000000000000, 1.000000000000000000 ),
 .UNSPECIFIED. ) 
 GEOMETRIC_REPRESENTATION_ITEM ( )  RATIONAL_B_SPLINE_SURFACE ( (
 ( 1.000000000000000000, 0.7071067811865425767, 1.000000000000000000),
 ( 1.000000000000000000, 0.7073403273941961666, 1.000000000000000000),
 ( 1.000000000000000000, 0.7061401876396929955, 1.000000000000000000),
 ( 1.000000000000000000, 0.7010830952601875277, 1.000000000000000000),
 ( 1.000000000000000000, 0.6972252234842747365, 1.000000000000000000),
 ( 1.000000000000000000, 0.6921057963906817045, 1.000000000000000000) ) ) 
 REPRESENTATION_ITEM ( '' )  SURFACE ( )  );
#6980 = LINE ( 'NONE', #1032, #10356 ) ;
#6981 = FACE_OUTER_BOUND ( 'NONE', #7441, .T. ) ;
#6982 = DIRECTION ( 'NONE',  ( 0.000000000000000000, 1.000000000000000000, 0.000000000000000000 ) ) ;
#6983 = VERTEX_POINT ( 'NONE', #10310 ) ;
#6984 = FACE_OUTER_BOUND ( 'NONE', #12159, .T. ) ;
#6985 = VERTEX_POINT ( 'NONE', #15092 ) ;
#6986 = ORIENTED_EDGE ( 'NONE', *, *, #2313, .F. ) ;
#6987 = EDGE_LOOP ( 'NONE', ( #4206, #7580, #14968, #13384 ) ) ;
#6988 = EDGE_CURVE ( 'NONE', #8322, #12221, #14853, .T. ) ;
#6989 = CIRCLE ( 'NONE', #11200, 0.5590551181102362266 ) ;
#6990 = DIRECTION ( 'NONE',  ( 0.000000000000000000, -1.734723475976802677E-14, 1.000000000000000000 ) ) ;
#6991 = CARTESIAN_POINT ( 'NONE',  ( 0.09842519685044806566, -0.4921259842519685179, -0.2482618547481154347 ) ) ;
#6992 = CARTESIAN_POINT ( 'NONE',  ( -0.03967601873944331947, 0.1701129415451921312, -0.04931034005880049337 ) ) ;
#6993 = CARTESIAN_POINT ( 'NONE',  ( 1.137795275590550936, 4.097147066950659020E-16, -0.02952755905511811330 ) ) ;
#6994 = DIRECTION ( 'NONE',  ( 0.000000000000000000, 0.000000000000000000, 1.000000000000000000 ) ) ;
#6995 = CARTESIAN_POINT ( 'NONE',  ( 0.05905511811029064834, -0.09842519685039370636, -0.5870514566507987197 ) ) ;
#6996 = ORIENTED_EDGE ( 'NONE', *, *, #13039, .F. ) ;
#6997 = SPHERICAL_SURFACE ( 'NONE', #11937, 0.003937007874015747977 ) ;
#6998 = DIRECTION ( 'NONE',  ( 0.5000000000000003331, 0.000000000000000000, -0.8660254037844387076 ) ) ;
#6999 = DIRECTION ( 'NONE',  ( 0.000000000000000000, 1.000000000000000000, 0.000000000000000000 ) ) ;
#7000 = EDGE_LOOP ( 'NONE', ( #11255, #4988, #762, #943 ) ) ;
#7001 = ORIENTED_EDGE ( 'NONE', *, *, #950, .F. ) ;
#7002 =( REPRESENTATION_RELATIONSHIP ('NONE','NONE', #8904, #11075 ) REPRESENTATION_RELATIONSHIP_WITH_TRANSFORMATION ( #9510 )SHAPE_REPRESENTATION_RELATIONSHIP( ) );
#7003 = DIRECTION ( 'NONE',  ( 0.5000000000000001110, 0.000000000000000000, 0.8660254037844384856 ) ) ;
#7004 = VERTEX_POINT ( 'NONE', #7257 ) ;
#7005 = ORIENTED_EDGE ( 'NONE', *, *, #11420, .T. ) ;
#7006 = EDGE_CURVE ( 'NONE', #4717, #10145, #14476, .T. ) ;
#7007 = ORIENTED_EDGE ( 'NONE', *, *, #4754, .F. ) ;
#7008 = DIRECTION ( 'NONE',  ( 0.000000000000000000, 0.000000000000000000, 1.000000000000000000 ) ) ;
#7009 = EDGE_CURVE ( 'NONE', #7744, #4401, #6326, .T. ) ;
#7010 = LINE ( 'NONE', #2067, #2345 ) ;
#7011 = DIRECTION ( 'NONE',  ( -0.000000000000000000, -0.000000000000000000, -1.000000000000000000 ) ) ;
#7012 = DIRECTION ( 'NONE',  ( -0.4999999999999971134, 0.000000000000000000, -0.8660254037844402619 ) ) ;
#7013 = CARTESIAN_POINT ( 'NONE',  ( 0.5610236220472175628, -0.1023622047244094474, 0.2102555114175294892 ) ) ;
#7014 = EDGE_CURVE ( 'NONE', #4871, #12169, #9602, .T. ) ;
#7015 = CARTESIAN_POINT ( 'NONE',  ( -0.07874015748031501505, 0.1442356988431299225, -0.03937007874015747977 ) ) ;
#7016 = CARTESIAN_POINT ( 'NONE',  ( 0.000000000000000000, 0.4133858267716535306, 0.000000000000000000 ) ) ;
#7017 = DIRECTION ( 'NONE',  ( 0.000000000000000000, 0.000000000000000000, 1.000000000000000000 ) ) ;
#7018 =( NAMED_UNIT ( * ) PLANE_ANGLE_UNIT ( ) SI_UNIT ( $, .RADIAN. ) );
#7019 = ORIENTED_EDGE ( 'NONE', *, *, #13615, .T. ) ;
#7020 = ORIENTED_EDGE ( 'NONE', *, *, #9712, .T. ) ;
#7021 = EDGE_LOOP ( 'NONE', ( #6621, #1794, #14270, #3319 ) ) ;
#7022 = EDGE_LOOP ( 'NONE', ( #13111, #7985, #304, #6072 ) ) ;
#7023 = EDGE_CURVE ( 'NONE', #1166, #4548, #2544, .T. ) ;
#7024 = EDGE_CURVE ( 'NONE', #6020, #13296, #1342, .T. ) ;
#7025 = CARTESIAN_POINT ( 'NONE',  ( -1.584115185264708403, 0.1296286773226378863, -0.05905511811023624047 ) ) ;
#7026 = LINE ( 'NONE', #9300, #15199 ) ;
#7027 = EDGE_CURVE ( 'NONE', #13379, #3964, #15361, .T. ) ;
#7028 = FACE_OUTER_BOUND ( 'NONE', #14020, .T. ) ;
#7029 = EDGE_CURVE ( 'NONE', #6744, #3640, #11896, .T. ) ;
#7030 = DIRECTION ( 'NONE',  ( -0.8660254037844383745, 0.000000000000000000, -0.5000000000000003331 ) ) ;
#7031 = FACE_OUTER_BOUND ( 'NONE', #9294, .T. ) ;
#7032 = ORIENTED_EDGE ( 'NONE', *, *, #277, .T. ) ;
#7033 = CARTESIAN_POINT ( 'NONE',  ( 0.03886060139087953863, 0.06736074103232488064, 0.08219815605943972536 ) ) ;
#7034 = LINE ( 'NONE', #8138, #14409 ) ;
#7035 = PRODUCT_DEFINITION_SHAPE ( 'NONE', 'NONE',  #15483 ) ;
#7036 = ORIENTED_EDGE ( 'NONE', *, *, #2702, .F. ) ;
#7037 = ORIENTED_EDGE ( 'NONE', *, *, #8348, .F. ) ;
#7038 = ORIENTED_EDGE ( 'NONE', *, *, #9316, .T. ) ;
#7039 = DIRECTION ( 'NONE',  ( 1.000000000000000000, -0.000000000000000000, -0.000000000000000000 ) ) ;
#7040 = FACE_OUTER_BOUND ( 'NONE', #1049, .T. ) ;
#7041 = DIRECTION ( 'NONE',  ( 0.4999999999999979461, 0.000000000000000000, 0.8660254037844398178 ) ) ;
#7042 = EDGE_CURVE ( 'NONE', #9959, #13232, #10605, .T. ) ;
#7043 = CYLINDRICAL_SURFACE ( 'NONE', #1235, 0.003937007874015758385 ) ;
#7044 = LINE ( 'NONE', #11831, #4719 ) ;
#7045 = LINE ( 'NONE', #12003, #15405 ) ;
#7046 = VERTEX_POINT ( 'NONE', #9701 ) ;
#7047 = CYLINDRICAL_SURFACE ( 'NONE', #2921, 0.2362204724409451007 ) ;
#7048 = CARTESIAN_POINT ( 'NONE',  ( 0.000000000000000000, -0.09842519685039370636, 0.000000000000000000 ) ) ;
#7049 = SPHERICAL_SURFACE ( 'NONE', #4092, 0.003937007874015747977 ) ;
#7050 = ORIENTED_EDGE ( 'NONE', *, *, #878, .T. ) ;
#7051 = EDGE_CURVE ( 'NONE', #7115, #9504, #3842, .T. ) ;
#7052 = ORIENTED_EDGE ( 'NONE', *, *, #11748, .F. ) ;
#7053 = ORIENTED_EDGE ( 'NONE', *, *, #49, .T. ) ;
#7054 = DIMENSIONAL_EXPONENTS ( 1.000000000000000000, 0.000000000000000000, 0.000000000000000000, 0.000000000000000000, 0.000000000000000000, 0.000000000000000000, 0.000000000000000000 ) ;
#7055 = ORIENTED_EDGE ( 'NONE', *, *, #4321, .F. ) ;
#7056 = ORIENTED_EDGE ( 'NONE', *, *, #7107, .F. ) ;
#7057 = CARTESIAN_POINT ( 'NONE',  ( 0.05905511811023625435, 2.637795275590551825, 0.03937007874015747977 ) ) ;
#7058 = CARTESIAN_POINT ( 'NONE',  ( 0.05314960629918537988, -0.09842519685039370636, -0.09205781851247189784 ) ) ;
#7059 = CARTESIAN_POINT ( 'NONE',  ( -1.607347794336916103, 0.09769578488571013797, -0.07191154586943661331 ) ) ;
#7060 = FACE_OUTER_BOUND ( 'NONE', #10971, .T. ) ;
#7061 = CARTESIAN_POINT ( 'NONE',  ( -0.6923203342731879539, -0.2952755905511811330, -0.2821984354013215568 ) ) ;
#7062 = DIRECTION ( 'NONE',  ( 0.8660254037844433705, 0.000000000000000000, 0.4999999999999918954 ) ) ;
#7063 = ORIENTED_EDGE ( 'NONE', *, *, #4526, .F. ) ;
#7064 = CARTESIAN_POINT ( 'NONE',  ( 0.4121618538092042261, -0.2952755905511811330, 0.1243101294532688583 ) ) ;
#7065 = CARTESIAN_POINT ( 'NONE',  ( -0.1023622047242992161, -0.2952755905511811330, -0.4190977005962941981 ) ) ;
#7066 = FACE_OUTER_BOUND ( 'NONE', #4193, .T. ) ;
#7067 = ADVANCED_FACE ( 'NONE', ( #3572, #13285 ), #1469, .F. ) ;
#7068 = DIRECTION ( 'NONE',  ( -0.8660254037844427044, 0.000000000000000000, -0.4999999999999929501 ) ) ;
#7069 = ORIENTED_EDGE ( 'NONE', *, *, #13638, .T. ) ;
#7070 = DIRECTION ( 'NONE',  ( -0.000000000000000000, -1.000000000000000000, -0.000000000000000000 ) ) ;
#7071 = ORIENTED_EDGE ( 'NONE', *, *, #12010, .T. ) ;
#7072 = ORIENTED_EDGE ( 'NONE', *, *, #128, .F. ) ;
#7073 = ORIENTED_EDGE ( 'NONE', *, *, #15440, .T. ) ;
#7074 = CARTESIAN_POINT ( 'NONE',  ( -2.090051324975654268, -1.858423098537180129, 0.08664193191037310171 ) ) ;
#7075 = CIRCLE ( 'NONE', #2318, 0.01968503937007875723 ) ;
#7076 = CIRCLE ( 'NONE', #11321, 0.003937007874015741038 ) ;
#7077 = CARTESIAN_POINT ( 'NONE',  ( 0.000000000000000000, 0.03149606299212599769, -0.1653543307086614012 ) ) ;
#7078 = CARTESIAN_POINT ( 'NONE',  ( -1.932774803826795784, -2.849358176375062612, 0.1599454478317489103 ) ) ;
#7079 = CIRCLE ( 'NONE', #336, 0.03937007874015752140 ) ;
#7080 = CARTESIAN_POINT ( 'NONE',  ( -1.607606114292110977, 0.09732815221480034529, 0.08366141732283462196 ) ) ;
#7081 = DIRECTION ( 'NONE',  ( 0.8660254037844388186, 0.000000000000000000, -0.4999999999999996669 ) ) ;
#7082 = LINE ( 'NONE', #11737, #13364 ) ;
#7083 = B_SPLINE_CURVE_WITH_KNOTS ( 'NONE', 3,
 ( #6802, #11834, #5710, #8062, #14028, #1031 ),
 .UNSPECIFIED., .F., .F.,
 ( 4, 2, 4 ),
 ( 0.000000000000000000, 0.0001791382075655873222, 0.0003582764151311746445 ),
 .UNSPECIFIED. ) ;
#7084 = DIRECTION ( 'NONE',  ( 0.000000000000000000, 0.000000000000000000, -1.000000000000000000 ) ) ;
#7085 = CYLINDRICAL_SURFACE ( 'NONE', #8420, 0.003937007874015749712 ) ;
#7086 = AXIS2_PLACEMENT_3D ( 'NONE', #11779, #1042, #13182 ) ;
#7087 = EDGE_CURVE ( 'NONE', #14162, #5049, #3509, .T. ) ;
#7088 = ORIENTED_EDGE ( 'NONE', *, *, #1581, .T. ) ;
#7089 = AXIS2_PLACEMENT_3D ( 'NONE', #2994, #14989, #9026 ) ;
#7090 = EDGE_LOOP ( 'NONE', ( #8342, #5555, #10815 ) ) ;
#7091 = CIRCLE ( 'NONE', #5074, 0.04330708661417331101 ) ;
#7092 = ORIENTED_EDGE ( 'NONE', *, *, #13418, .T. ) ;
#7093 = ORIENTED_EDGE ( 'NONE', *, *, #14318, .T. ) ;
#7094 = EDGE_CURVE ( 'NONE', #8301, #12057, #8599, .T. ) ;
#7095 = DIRECTION ( 'NONE',  ( 1.224646799147353207E-16, 1.000000000000000000, 0.000000000000000000 ) ) ;
#7096 = AXIS2_PLACEMENT_3D ( 'NONE', #12991, #11813, #14005 ) ;
#7097 = VECTOR ( 'NONE', #12743, 39.37007874015748143 ) ;
#7098 = CARTESIAN_POINT ( 'NONE',  ( -0.007954450877556133725, 0.1525563742223925434, 0.01590295032064549530 ) ) ;
#7099 = CARTESIAN_POINT ( 'NONE',  ( -1.568343923620152180, 0.1178486908565801600, -0.05905511811023622659 ) ) ;
#7100 = AXIS2_PLACEMENT_3D ( 'NONE', #6638, #13623, #848 ) ;
#7101 = DIRECTION ( 'NONE',  ( 0.000000000000000000, 1.000000000000000000, 0.000000000000000000 ) ) ;
#7102 = CIRCLE ( 'NONE', #9376, 0.03937007874015751446 ) ;
#7103 = FACE_OUTER_BOUND ( 'NONE', #7454, .T. ) ;
#7104 = ORIENTED_EDGE ( 'NONE', *, *, #13311, .F. ) ;
#7105 = SURFACE_SIDE_STYLE ('',( #2321 ) ) ;
#7106 = CARTESIAN_POINT ( 'NONE',  ( 0.000000000000000000, 2.393700787401575436, -0.5511811023622046335 ) ) ;
#7107 = EDGE_CURVE ( 'NONE', #14143, #5321, #4090, .T. ) ;
#7108 = EDGE_CURVE ( 'NONE', #4737, #9204, #4592, .T. ) ;
#7109 = ORIENTED_EDGE ( 'NONE', *, *, #12230, .F. ) ;
#7110 = ORIENTED_EDGE ( 'NONE', *, *, #10583, .F. ) ;
#7111 = CIRCLE ( 'NONE', #6342, 0.003937007874015758385 ) ;
#7112 = TOROIDAL_SURFACE ( 'NONE', #7860, 0.04330708661417328326, 0.003937007874015747977 ) ;
#7113 = AXIS2_PLACEMENT_3D ( 'NONE', #860, #952, #3220 ) ;
#7114 = EDGE_CURVE ( 'NONE', #1873, #7239, #12848, .T. ) ;
#7115 = VERTEX_POINT ( 'NONE', #8669 ) ;
#7116 = CIRCLE ( 'NONE', #13875, 0.01968503937007871907 ) ;
#7117 = CARTESIAN_POINT ( 'NONE',  ( 0.000000000000000000, 0.07874015748031495954, 0.000000000000000000 ) ) ;
#7118 = FACE_OUTER_BOUND ( 'NONE', #12739, .T. ) ;
#7119 = CARTESIAN_POINT ( 'NONE',  ( -1.950386452976718976, -2.919842877483835419, -0.07215111381683911307 ) ) ;
#7120 = DIRECTION ( 'NONE',  ( 0.000000000000000000, 1.000000000000000000, 0.000000000000000000 ) ) ;
#7121 = CARTESIAN_POINT ( 'NONE',  ( -2.464375602680784816, 0.7077922088437120784, -0.1033464566929134798 ) ) ;
#7122 = AXIS2_PLACEMENT_3D ( 'NONE', #509, #13567, #437 ) ;
#7123 = CARTESIAN_POINT ( 'NONE',  ( 0.000000000000000000, 1.661417322834646049, -0.5984251968503937480 ) ) ;
#7124 = AXIS2_PLACEMENT_3D ( 'NONE', #6590, #7624, #12420 ) ;
#7125 = CARTESIAN_POINT ( 'NONE',  ( -1.964126537190518107, -2.749515453455440905, 0.1756903148397124803 ) ) ;
#7126 = AXIS2_PLACEMENT_3D ( 'NONE', #13863, #6794, #5772 ) ;
#7127 = ORIENTED_EDGE ( 'NONE', *, *, #7425, .F. ) ;
#7128 = CARTESIAN_POINT ( 'NONE',  ( -1.948440798307840227, -2.924613150232347802, -0.06209002033771690576 ) ) ;
#7129 = DIRECTION ( 'NONE',  ( -4.292327424963297008E-16, 1.000000000000000000, 2.478176394252599876E-16 ) ) ;
#7130 = AXIS2_PLACEMENT_3D ( 'NONE', #10314, #10638, #15424 ) ;
#7131 = CARTESIAN_POINT ( 'NONE',  ( 0.5424655050177952242, 1.338877451511696570, 0.2450016286721640457 ) ) ;
#7132 = EDGE_CURVE ( 'NONE', #11777, #10377, #3608, .T. ) ;
#7133 = DIRECTION ( 'NONE',  ( 0.000000000000000000, 0.000000000000000000, -1.000000000000000000 ) ) ;
#7134 = EDGE_LOOP ( 'NONE', ( #9468, #11139, #2043, #5681 ) ) ;
#7135 = ADVANCED_FACE ( 'NONE', ( #8577 ), #226, .F. ) ;
#7136 = ORIENTED_EDGE ( 'NONE', *, *, #4674, .F. ) ;
#7138 = VERTEX_POINT ( 'NONE', #4262 ) ;
#7137 = CIRCLE ( 'NONE', #879, 0.5905511811023621549 ) ;
#7139 = AXIS2_PLACEMENT_3D ( 'NONE', #12314, #13648, #10415 ) ;
#7140 = ORIENTED_EDGE ( 'NONE', *, *, #10813, .F. ) ;
#7141 = AXIS2_PLACEMENT_3D ( 'NONE', #1255, #3752, #8294 ) ;
#7142 = DIRECTION ( 'NONE',  ( 0.000000000000000000, -1.000000000000000000, 0.000000000000000000 ) ) ;
#7143 = AXIS2_PLACEMENT_3D ( 'NONE', #4979, #9777, #14481 ) ;
#7144 = ADVANCED_FACE ( 'NONE', ( #2949 ), #519, .F. ) ;
#7145 = CARTESIAN_POINT ( 'NONE',  ( -0.06692913385815735250, -0.1023622047244094474, -0.5909884645248143498 ) ) ;
#7146 = CARTESIAN_POINT ( 'NONE',  ( -0.05905511811023622659, 1.043292445042268257, -0.5949473527966270270 ) ) ;
#7147 = CONTEXT_DEPENDENT_SHAPE_REPRESENTATION ( #4087, #13445 ) ;
#7148 = DIRECTION ( 'NONE',  ( -0.000000000000000000, -0.000000000000000000, -1.000000000000000000 ) ) ;
#7149 = CARTESIAN_POINT ( 'NONE',  ( -0.2939481552201428372, -0.2952755905511811330, 0.2424480883318111957 ) ) ;
#7150 = ORIENTED_EDGE ( 'NONE', *, *, #6835, .F. ) ;
#7151 = DIRECTION ( 'NONE',  ( 0.000000000000000000, 0.000000000000000000, -1.000000000000000000 ) ) ;
#7152 = CYLINDRICAL_SURFACE ( 'NONE', #13653, 0.003937007874015749712 ) ;
#7153 = AXIS2_PLACEMENT_3D ( 'NONE', #10994, #12321, #4173 ) ;
#7154 = COLOUR_RGB ( '',0.7921568627450980005, 0.8196078431372548767, 0.9333333333333333481 ) ;
#7155 = CARTESIAN_POINT ( 'NONE',  ( 0.09842519685044817668, -0.2952755905511811330, -0.4584677793364516640 ) ) ;
#7156 = VECTOR ( 'NONE', #11380, 39.37007874015748143 ) ;
#7157 = AXIS2_PLACEMENT_3D ( 'NONE', #9596, #215, #8732 ) ;
#7158 = ORIENTED_EDGE ( 'NONE', *, *, #10934, .T. ) ;
#7159 = ORIENTED_EDGE ( 'NONE', *, *, #11600, .F. ) ;
#7160 = EDGE_CURVE ( 'NONE', #11226, #115, #13353, .T. ) ;
#7161 = ORIENTED_EDGE ( 'NONE', *, *, #6478, .T. ) ;
#7162 = ORIENTED_EDGE ( 'NONE', *, *, #3235, .F. ) ;
#7163 = ORIENTED_EDGE ( 'NONE', *, *, #11563, .F. ) ;
#7164 = DIRECTION ( 'NONE',  ( 1.000000000000000000, 0.000000000000000000, 0.000000000000000000 ) ) ;
#7165 = EDGE_CURVE ( 'NONE', #776, #14049, #3970, .T. ) ;
#7166 = DIRECTION ( 'NONE',  ( 0.8660254037844399289, 0.000000000000000000, 0.4999999999999975575 ) ) ;
#7167 = CARTESIAN_POINT ( 'NONE',  ( 0.5576140732134206024, -0.4881889763779528324, 0.2082870074805215910 ) ) ;
#7168 = CARTESIAN_POINT ( 'NONE',  ( -0.1614173228351908074, 35.52269057326158475, -0.4190977005993389848 ) ) ;
#7169 = DIRECTION ( 'NONE',  ( 0.000000000000000000, 0.000000000000000000, -1.000000000000000000 ) ) ;
#7170 = AXIS2_PLACEMENT_3D ( 'NONE', #3076, #12496, #7622 ) ;
#7171 = CARTESIAN_POINT ( 'NONE',  ( -1.107198012490790306, -0.06846922848666056605, 0.03937007874015747977 ) ) ;
#7172 = DIRECTION ( 'NONE',  ( 0.000000000000000000, 1.000000000000000000, 0.000000000000000000 ) ) ;
#7173 = DIRECTION ( 'NONE',  ( -1.000000000000000000, 0.000000000000000000, -8.673617379884028570E-16 ) ) ;
#7174 = CARTESIAN_POINT ( 'NONE',  ( 0.7455328141524918406, 1.338582677165354395, 0.3622425942646915753 ) ) ;
#7175 = DIRECTION ( 'NONE',  ( 0.000000000000000000, 0.000000000000000000, 1.000000000000000000 ) ) ;
#7176 = DIRECTION ( 'NONE',  ( -0.000000000000000000, -1.000000000000000000, -0.000000000000000000 ) ) ;
#7177 = CIRCLE ( 'NONE', #13931, 0.003937007874015749712 ) ;
#7178 = VERTEX_POINT ( 'NONE', #1838 ) ;
#7179 = EDGE_LOOP ( 'NONE', ( #7293, #1829, #471, #11511 ) ) ;
#7180 = EDGE_LOOP ( 'NONE', ( #10935, #3252, #7161, #2959 ) ) ;
#7181 = CIRCLE ( 'NONE', #9185, 0.01968503937007880233 ) ;
#7182 = VERTEX_POINT ( 'NONE', #11244 ) ;
#7183 = AXIS2_PLACEMENT_3D ( 'NONE', #7949, #3411, #4496 ) ;
#7184 = DIRECTION ( 'NONE',  ( 0.000000000000000000, -1.000000000000000000, -0.000000000000000000 ) ) ;
#7185 = CIRCLE ( 'NONE', #11222, 0.6614173228346456046 ) ;
#7186 = CARTESIAN_POINT ( 'NONE',  ( -0.4815353412745217998, 1.340095897400991110, 0.3474236500605538125 ) ) ;
#7187 = AXIS2_PLACEMENT_3D ( 'NONE', #11425, #1948, #6541 ) ;
#7188 = DIRECTION ( 'NONE',  ( 0.7402970580929162381, 0.6722799013647318134, -1.027368548696278368E-14 ) ) ;
#7189 = LINE ( 'NONE', #8512, #3156 ) ;
#7190 = DIRECTION ( 'NONE',  ( 0.000000000000000000, 0.000000000000000000, -1.000000000000000000 ) ) ;
#7191 = CIRCLE ( 'NONE', #451, 0.003937007874015758385 ) ;
#7192 = DIRECTION ( 'NONE',  ( -0.000000000000000000, 0.000000000000000000, 1.000000000000000000 ) ) ;
#7193 = ORIENTED_EDGE ( 'NONE', *, *, #10480, .F. ) ;
#7194 = DIRECTION ( 'NONE',  ( -0.000000000000000000, -0.000000000000000000, 1.000000000000000000 ) ) ;
#7195 = LINE ( 'NONE', #11757, #638 ) ;
#7196 = AXIS2_PLACEMENT_3D ( 'NONE', #10519, #13093, #11943 ) ;
#7197 = ORIENTED_EDGE ( 'NONE', *, *, #10361, .T. ) ;
#7198 = ORIENTED_EDGE ( 'NONE', *, *, #3796, .F. ) ;
#7199 = AXIS2_PLACEMENT_3D ( 'NONE', #3707, #13256, #12077 ) ;
#7200 = VERTEX_POINT ( 'NONE', #12574 ) ;
#7201 = AXIS2_PLACEMENT_3D ( 'NONE', #1282, #5092, #10819 ) ;
#7202 = DIRECTION ( 'NONE',  ( 0.000000000000000000, 0.000000000000000000, -1.000000000000000000 ) ) ;
#7203 = EDGE_CURVE ( 'NONE', #1544, #9167, #3342, .T. ) ;
#7204 = LINE ( 'NONE', #1321, #11402 ) ;
#7205 = EDGE_CURVE ( 'NONE', #6733, #14099, #10337, .T. ) ;
#7206 = LINE ( 'NONE', #5774, #9128 ) ;
#7207 = CARTESIAN_POINT ( 'NONE',  ( 0.000000000000000000, 0.000000000000000000, 0.000000000000000000 ) ) ;
#7208 = CARTESIAN_POINT ( 'NONE',  ( -0.4769054117961255002, -0.09842519685039372024, 0.3480785096661502265 ) ) ;
#7210 = AXIS2_PLACEMENT_3D ( 'NONE', #5082, #13487, #262 ) ;
#7209 = CARTESIAN_POINT ( 'NONE',  ( -1.253866366384063902, 0.1355266887446167634, 0.05905511811023622659 ) ) ;
#7211 = DIRECTION ( 'NONE',  ( 1.000000000000000000, 0.000000000000000000, 1.224646799147353207E-16 ) ) ;
#7212 = ORIENTED_EDGE ( 'NONE', *, *, #13174, .T. ) ;
#7213 = CARTESIAN_POINT ( 'NONE',  ( -1.983894532046819537, -2.833993371773555037, 0.1480485534673108006 ) ) ;
#7214 = EDGE_CURVE ( 'NONE', #9905, #8101, #13682, .T. ) ;
#7215 = FACE_OUTER_BOUND ( 'NONE', #1646, .T. ) ;
#7216 = DIRECTION ( 'NONE',  ( 0.000000000000000000, 1.000000000000000000, -0.000000000000000000 ) ) ;
#7217 = VERTEX_POINT ( 'NONE', #8743 ) ;
#7218 = ORIENTED_EDGE ( 'NONE', *, *, #15282, .F. ) ;
#7219 = AXIS2_PLACEMENT_3D ( 'NONE', #6172, #3759, #7508 ) ;
#7220 = FACE_OUTER_BOUND ( 'NONE', #4498, .T. ) ;
#7221 = ADVANCED_FACE ( 'NONE', ( #5202 ), #6521, .T. ) ;
#7222 = DIRECTION ( 'NONE',  ( -0.000000000000000000, -1.000000000000000000, 0.000000000000000000 ) ) ;
#7223 = EDGE_CURVE ( 'NONE', #8290, #9755, #11349, .T. ) ;
#7224 = DIRECTION ( 'NONE',  ( 0.000000000000000000, 0.000000000000000000, -1.000000000000000000 ) ) ;
#7225 = DIRECTION ( 'NONE',  ( -0.8660254037844385966, 0.000000000000000000, -0.5000000000000003331 ) ) ;
#7226 = ITEM_DEFINED_TRANSFORMATION ( 'NONE', 'NONE', #12130,  #11481 ) ;
#7227 = CARTESIAN_POINT ( 'NONE',  ( 0.1062992125984796865, -0.09448818897637796532, -0.5870514566507987197 ) ) ;
#7228 = CARTESIAN_POINT ( 'NONE',  ( -1.437672431148612429, -0.06355280397547365123, 0.08366141732283458032 ) ) ;
#7229 = DIRECTION ( 'NONE',  ( -0.000000000000000000, -0.000000000000000000, -1.000000000000000000 ) ) ;
#7230 = ORIENTED_EDGE ( 'NONE', *, *, #8495, .T. ) ;
#7231 = CARTESIAN_POINT ( 'NONE',  ( -0.08151194962748883888, 0.1637246173173400876, 0.03937007874015747977 ) ) ;
#7232 = EDGE_CURVE ( 'NONE', #13241, #161, #5829, .T. ) ;
#7233 = DIRECTION ( 'NONE',  ( -0.000000000000000000, 1.000000000000000000, -0.000000000000000000 ) ) ;
#7234 = CARTESIAN_POINT ( 'NONE',  ( -0.04489327544264908737, -0.1650454269528150719, 0.05194604157257243227 ) ) ;
#7235 = ORIENTED_EDGE ( 'NONE', *, *, #11997, .T. ) ;
#7236 = AXIS2_PLACEMENT_3D ( 'NONE', #10426, #10733, #9559 ) ;
#7237 = ORIENTED_EDGE ( 'NONE', *, *, #4982, .F. ) ;
#7238 = ORIENTED_EDGE ( 'NONE', *, *, #944, .F. ) ;
#7239 = VERTEX_POINT ( 'NONE', #681 ) ;
#7240 = CARTESIAN_POINT ( 'NONE',  ( -1.591501945092674175, 0.08600752902535276079, 0.08366141732283462196 ) ) ;
#7241 = DIRECTION ( 'NONE',  ( -1.000000000000000000, -0.000000000000000000, 0.000000000000000000 ) ) ;
#7242 = CARTESIAN_POINT ( 'NONE',  ( -1.904663734566028888, -2.930783973356453576, -0.08012620074318213548 ) ) ;
#7243 = DIRECTION ( 'NONE',  ( 1.471276157853479814E-16, 0.8642424528470445955, -0.5030755238499721171 ) ) ;
#7244 = CARTESIAN_POINT ( 'NONE',  ( 0.4769054117961250561, -0.4881889763779528324, 0.3480785096661500599 ) ) ;
#7245 = B_SPLINE_CURVE_WITH_KNOTS ( 'NONE', 3,
 ( #1793, #6546, #15427, #13143 ),
 .UNSPECIFIED., .F., .F.,
 ( 4, 4 ),
 ( 0.000000000000000000, 2.119993237936590205E-05 ),
 .UNSPECIFIED. ) ;
#7246 = CARTESIAN_POINT ( 'NONE',  ( 0.000000000000000000, 1.385826771653543510, 0.000000000000000000 ) ) ;
#7247 = CARTESIAN_POINT ( 'NONE',  ( 0.000000000000000000, 0.07480314960629921850, 0.000000000000000000 ) ) ;
#7248 = EDGE_CURVE ( 'NONE', #2367, #3987, #7336, .T. ) ;
#7249 = DIRECTION ( 'NONE',  ( 1.504632769052528010E-28, -8.673617379884035472E-15, -1.000000000000000000 ) ) ;
#7250 = DIRECTION ( 'NONE',  ( 0.000000000000000000, -0.000000000000000000, 1.000000000000000000 ) ) ;
#7251 = DIRECTION ( 'NONE',  ( 1.000000000000000000, 0.000000000000000000, 0.000000000000000000 ) ) ;
#7252 = ORIENTED_EDGE ( 'NONE', *, *, #9638, .T. ) ;
#7253 = ADVANCED_FACE ( 'NONE', ( #1531 ), #7640, .F. ) ;
#7254 = VERTEX_POINT ( 'NONE', #590 ) ;
#7255 = ORIENTED_EDGE ( 'NONE', *, *, #3073, .F. ) ;
#7256 = B_SPLINE_CURVE_WITH_KNOTS ( 'NONE', 3,
 ( #12078, #2289, #3479, #15467, #14514, #8254 ),
 .UNSPECIFIED., .F., .F.,
 ( 4, 2, 4 ),
 ( 2.168404344971008868E-19, 0.0003906568843879350858, 0.0007813137687758699547 ),
 .UNSPECIFIED. ) ;
#7257 = CARTESIAN_POINT ( 'NONE',  ( -1.431036756819010769, -0.02829858486107867874, 0.1033464566929133133 ) ) ;
#7258 = DIRECTION ( 'NONE',  ( -0.4999999999999966693, 0.000000000000000000, 0.8660254037844405950 ) ) ;
#7259 = FACE_OUTER_BOUND ( 'NONE', #38, .T. ) ;
#7260 = CARTESIAN_POINT ( 'NONE',  ( -0.3569402812043674933, -0.2952755905511811330, 0.1333425256503556200 ) ) ;
#7261 = DIRECTION ( 'NONE',  ( 0.000000000000000000, 0.000000000000000000, 1.000000000000000000 ) ) ;
#7262 = LINE ( 'NONE', #2487, #11135 ) ;
#7263 = DIRECTION ( 'NONE',  ( -0.000000000000000000, -1.000000000000000000, -0.000000000000000000 ) ) ;
#7264 = FACE_OUTER_BOUND ( 'NONE', #6536, .T. ) ;
#7265 = CARTESIAN_POINT ( 'NONE',  ( -0.1463103599444685599, -0.09842519685039370636, -0.08447232569917004219 ) ) ;
#7266 = ORIENTED_EDGE ( 'NONE', *, *, #9115, .T. ) ;
#7267 = ORIENTED_EDGE ( 'NONE', *, *, #2012, .T. ) ;
#7268 = ORIENTED_EDGE ( 'NONE', *, *, #10009, .F. ) ;
#7269 = DIRECTION ( 'NONE',  ( -0.8660254037844384856, 0.000000000000000000, -0.5000000000000003331 ) ) ;
#7270 = CARTESIAN_POINT ( 'NONE',  ( -1.593720380426979499, 0.1169877005562640487, 0.06604764719690611741 ) ) ;
#7271 = DIRECTION ( 'NONE',  ( 4.292327424963333000E-16, 1.000000000000000000, 2.478176394252540712E-16 ) ) ;
#7272 = CARTESIAN_POINT ( 'NONE',  ( -1.591501945092674175, 0.08600752902535263589, 0.08366141732283462196 ) ) ;
#7273 = DIRECTION ( 'NONE',  ( -0.000000000000000000, -1.000000000000000000, -0.000000000000000000 ) ) ;
#7274 = DIRECTION ( 'NONE',  ( 0.000000000000000000, 0.000000000000000000, 1.000000000000000000 ) ) ;
#7275 = CARTESIAN_POINT ( 'NONE',  ( -1.904045375254802996, -2.861202609515447026, 0.1539435876055646746 ) ) ;
#7276 = ORIENTED_EDGE ( 'NONE', *, *, #522, .F. ) ;
#7277 = CARTESIAN_POINT ( 'NONE',  ( -1.983904060594682051, -2.833967658977468052, -0.1480566138544802401 ) ) ;
#7278 = DIRECTION ( 'NONE',  ( 0.000000000000000000, 0.000000000000000000, -1.000000000000000000 ) ) ;
#7279 = CARTESIAN_POINT ( 'NONE',  ( 0.000000000000000000, 0.3228346456692913757, -0.7086614173228346081 ) ) ;
#7280 = VERTEX_POINT ( 'NONE', #9931 ) ;
#7281 = EDGE_CURVE ( 'NONE', #3157, #897, #7845, .T. ) ;
#7282 = ORIENTED_EDGE ( 'NONE', *, *, #8162, .T. ) ;
#7283 = EDGE_CURVE ( 'NONE', #14180, #15344, #101, .T. ) ;
#7284 = VERTEX_POINT ( 'NONE', #5348 ) ;
#7285 = DIRECTION ( 'NONE',  ( -1.000000000000000000, -0.000000000000000000, -3.614007241618347785E-16 ) ) ;
#7286 = EDGE_CURVE ( 'NONE', #6774, #11698, #6283, .T. ) ;
#7287 = CARTESIAN_POINT ( 'NONE',  ( -0.4591888763630547210, -0.4881889763779528324, 0.3787644491703232585 ) ) ;
#7288 = CARTESIAN_POINT ( 'NONE',  ( -0.06012940348033153637, 1.041728643793834674, -0.5902917039295723090 ) ) ;
#7289 = DIRECTION ( 'NONE',  ( -0.8660254037844388186, 0.000000000000000000, 0.4999999999999995559 ) ) ;
#7290 = ITEM_DEFINED_TRANSFORMATION ( 'NONE', 'NONE', #3120,  #11481 ) ;
#7291 = DIRECTION ( 'NONE',  ( 0.000000000000000000, -1.000000000000000000, 0.000000000000000000 ) ) ;
#7292 = DIRECTION ( 'NONE',  ( 0.000000000000000000, 0.000000000000000000, 1.000000000000000000 ) ) ;
#7293 = ORIENTED_EDGE ( 'NONE', *, *, #5359, .T. ) ;
#7294 = FACE_OUTER_BOUND ( 'NONE', #9362, .T. ) ;
#7295 = DIRECTION ( 'NONE',  ( -1.734723475976802677E-14, 0.000000000000000000, -1.000000000000000000 ) ) ;
#7296 = DIRECTION ( 'NONE',  ( 0.000000000000000000, 0.000000000000000000, -1.000000000000000000 ) ) ;
#7297 = ADVANCED_FACE ( 'NONE', ( #11165 ), #13857, .T. ) ;
#7298 = CARTESIAN_POINT ( 'NONE',  ( 0.000000000000000000, 1.035433070866142113, 0.000000000000000000 ) ) ;
#7299 = ADVANCED_FACE ( 'NONE', ( #14940 ), #10296, .T. ) ;
#7300 = ORIENTED_EDGE ( 'NONE', *, *, #10025, .T. ) ;
#7301 = ORIENTED_EDGE ( 'NONE', *, *, #7281, .T. ) ;
#7302 = ORIENTED_EDGE ( 'NONE', *, *, #7682, .F. ) ;
#7303 = ORIENTED_EDGE ( 'NONE', *, *, #3634, .T. ) ;
#7304 = ADVANCED_FACE ( 'NONE', ( #5510 ), #4341, .F. ) ;
#7305 = CARTESIAN_POINT ( 'NONE',  ( -0.07635964791965738074, -0.1878198040935885327, -0.03937007874015747977 ) ) ;
#7306 = CARTESIAN_POINT ( 'NONE',  ( -0.7796283024904574477, 1.190944881889763884, 0.3819276336347811607 ) ) ;
#7307 = DIRECTION ( 'NONE',  ( 0.8660254037844384856, 0.000000000000000000, -0.5000000000000004441 ) ) ;
#7308 = DIRECTION ( 'NONE',  ( 0.4932581959314710773, 0.8219459448134286417, 0.2847827522010255574 ) ) ;
#7309 = CARTESIAN_POINT ( 'NONE',  ( 0.1023622047244639455, -0.09842519685039372024, -0.5870514566507987197 ) ) ;
#7310 = CARTESIAN_POINT ( 'NONE',  ( -1.527714331928839098, 0.2380340132385416752, -0.05905511811023622659 ) ) ;
#7311 = DIRECTION ( 'NONE',  ( -0.000000000000000000, 0.000000000000000000, 1.000000000000000000 ) ) ;
#7312 = DIRECTION ( 'NONE',  ( 0.8660254037844464792, 0.000000000000000000, 0.4999999999999864553 ) ) ;
#7313 = CARTESIAN_POINT ( 'NONE',  ( -1.957251767099916107, -2.772329397582958599, 0.1771653543307079026 ) ) ;
#7314 = DIRECTION ( 'NONE',  ( -0.8660254037844405950, 0.000000000000000000, 0.4999999999999966693 ) ) ;
#7315 = ADVANCED_FACE ( 'NONE', ( #8106, #15315 ), #5582, .F. ) ;
#7316 = EDGE_LOOP ( 'NONE', ( #549, #5788, #9879, #402 ) ) ;
#7317 = ORIENTED_EDGE ( 'NONE', *, *, #4733, .T. ) ;
#7318 = TOROIDAL_SURFACE ( 'NONE', #5056, 0.5984251968503937480, 0.007874015748031495954 ) ;
#7319 = VERTEX_POINT ( 'NONE', #6932 ) ;
#7320 = AXIS2_PLACEMENT_3D ( 'NONE', #8913, #14858, #10239 ) ;
#7321 = EDGE_CURVE ( 'NONE', #4029, #11838, #3421, .T. ) ;
#7322 = DIRECTION ( 'NONE',  ( 0.000000000000000000, 0.000000000000000000, 1.000000000000000000 ) ) ;
#7323 = DIRECTION ( 'NONE',  ( -0.000000000000000000, -1.000000000000000000, -0.000000000000000000 ) ) ;
#7324 = EDGE_CURVE ( 'NONE', #4499, #1289, #7010, .T. ) ;
#7325 = CARTESIAN_POINT ( 'NONE',  ( 0.1552072824047652788, -0.09842519685039370636, -0.5870514566507987197 ) ) ;
#7326 = LINE ( 'NONE', #12212, #15335 ) ;
#7327 = CIRCLE ( 'NONE', #4091, 0.6614173228346456046 ) ;
#7328 = FACE_OUTER_BOUND ( 'NONE', #8491, .T. ) ;
#7329 = CARTESIAN_POINT ( 'NONE',  ( 0.06692913385832212347, -0.4881889763779528324, -0.5870514566507987197 ) ) ;
#7330 = DIRECTION ( 'NONE',  ( 3.476578583725179813E-16, 0.000000000000000000, -1.000000000000000000 ) ) ;
#7331 = DIRECTION ( 'NONE',  ( -0.000000000000000000, -1.000000000000000000, -0.000000000000000000 ) ) ;
#7332 = EDGE_LOOP ( 'NONE', ( #8687, #5364, #13542 ) ) ;
#7333 = VERTEX_POINT ( 'NONE', #15078 ) ;
#7334 = ORIENTED_EDGE ( 'NONE', *, *, #1659, .T. ) ;
#7335 = ORIENTED_EDGE ( 'NONE', *, *, #9108, .T. ) ;
#7336 = CIRCLE ( 'NONE', #9106, 0.007874015748031501158 ) ;
#7337 = CARTESIAN_POINT ( 'NONE',  ( -0.4815353412745563833, 0.000000000000000000, 0.3474236500605538680 ) ) ;
#7338 = CIRCLE ( 'NONE', #13110, 0.003937007874015780069 ) ;
#7339 = CIRCLE ( 'NONE', #6080, 0.003937007874015724558 ) ;
#7340 = CARTESIAN_POINT ( 'NONE',  ( 0.1552072824047652233, -0.003937007874015747977, -0.5870514566507987197 ) ) ;
#7341 = EDGE_CURVE ( 'NONE', #12059, #1905, #4850, .T. ) ;
#7342 = CARTESIAN_POINT ( 'NONE',  ( 0.000000000000000000, 0.5433070866141731514, 0.000000000000000000 ) ) ;
#7343 = CARTESIAN_POINT ( 'NONE',  ( 6.750021727583836750E-17, 0.3464566929133857109, 0.5511811023622046335 ) ) ;
#7344 = DIRECTION ( 'NONE',  ( 0.4999999999999922284, -0.000000000000000000, -0.8660254037844431485 ) ) ;
#7345 = CARTESIAN_POINT ( 'NONE',  ( -1.913759217590492057, -2.905162717098710434, 0.1179150947973677116 ) ) ;
#7346 = ORIENTED_EDGE ( 'NONE', *, *, #5942, .F. ) ;
#7347 = CARTESIAN_POINT ( 'NONE',  ( -0.6582248459352179060, -0.2952755905511811330, -0.3018834747714004840 ) ) ;
#7348 = CARTESIAN_POINT ( 'NONE',  ( 0.2939481552201435588, -0.2952755905511811330, 0.2424480883318115843 ) ) ;
#7349 = TOROIDAL_SURFACE ( 'NONE', #5601, 0.5433070866141731514, 0.007874015748031495954 ) ;
#7350 = CIRCLE ( 'NONE', #10114, 0.5905511811023621549 ) ;
#7351 = DIRECTION ( 'NONE',  ( -1.000000000000000000, 1.349229370204184172E-15, 0.000000000000000000 ) ) ;
#7352 = ORIENTED_EDGE ( 'NONE', *, *, #5284, .T. ) ;
#7353 = AXIS2_PLACEMENT_3D ( 'NONE', #15441, #4930, #8296 ) ;
#7354 = ORIENTED_EDGE ( 'NONE', *, *, #13235, .F. ) ;
#7355 = AXIS2_PLACEMENT_3D ( 'NONE', #12463, #7747, #626 ) ;
#7356 = CIRCLE ( 'NONE', #2108, 0.003937007874015724558 ) ;
#7357 = AXIS2_PLACEMENT_3D ( 'NONE', #6208, #2533, #280 ) ;
#7358 = ORIENTED_EDGE ( 'NONE', *, *, #15293, .F. ) ;
#7359 = LINE ( 'NONE', #6707, #9342 ) ;
#7360 = CIRCLE ( 'NONE', #1374, 0.01968503937007870172 ) ;
#7361 = VECTOR ( 'NONE', #13754, 39.37007874015748143 ) ;
#7362 = CIRCLE ( 'NONE', #7626, 0.04330708661417331101 ) ;
#7363 = CIRCLE ( 'NONE', #9386, 0.5590551181102362266 ) ;
#7364 = LINE ( 'NONE', #12164, #8354 ) ;
#7365 = DIRECTION ( 'NONE',  ( 1.000000000000000000, 0.000000000000000000, -0.000000000000000000 ) ) ;
#7366 = DIRECTION ( 'NONE',  ( -0.000000000000000000, -1.000000000000000000, -0.000000000000000000 ) ) ;
#7367 = CIRCLE ( 'NONE', #2627, 0.003937007874015750579 ) ;
#7368 = DIRECTION ( 'NONE',  ( -4.292327424963298981E-16, 1.000000000000000000, 2.478176394252600369E-16 ) ) ;
#7369 = EDGE_LOOP ( 'NONE', ( #11485, #10745, #6883, #4796 ) ) ;
#7370 = DIRECTION ( 'NONE',  ( 0.000000000000000000, 0.000000000000000000, 1.000000000000000000 ) ) ;
#7371 = LINE ( 'NONE', #4076, #1851 ) ;
#7372 = DIRECTION ( 'NONE',  ( 0.000000000000000000, 0.000000000000000000, -1.000000000000000000 ) ) ;
#7373 = DIRECTION ( 'NONE',  ( 0.000000000000000000, 0.000000000000000000, -1.000000000000000000 ) ) ;
#7374 = EDGE_CURVE ( 'NONE', #7659, #6576, #3844, .T. ) ;
#7375 =( LENGTH_UNIT ( ) NAMED_UNIT ( * ) SI_UNIT ( $, .METRE. ) );
#7376 = TOROIDAL_SURFACE ( 'NONE', #13635, 0.04527559055118110520, 0.005905511811023621965 ) ;
#7377 = AXIS2_PLACEMENT_3D ( 'NONE', #10321, #2021, #6719 ) ;
#7378 = AXIS2_PLACEMENT_3D ( 'NONE', #9722, #14493, #8522 ) ;
#7379 = ORIENTED_EDGE ( 'NONE', *, *, #1552, .F. ) ;
#7380 =( BOUNDED_SURFACE ( )  B_SPLINE_SURFACE ( 3, 2, ( 
 ( #12276, #3025, #11313 ),
 ( #6608, #1702, #7549 ),
 ( #11248, #12342, #1619 ),
 ( #13452, #6379, #5273 ),
 ( #13686, #11407, #11170 ),
 ( #524, #10067, #14851 ),
 ( #10236, #8909, #12512 ),
 ( #1770, #6526, #5355 ),
 ( #8988, #7791, #12579 ),
 ( #2720, #10522, #6694 ),
 ( #12667, #11712, #3097 ),
 ( #7877, #5726, #1929 ),
 ( #978, #4268, #9055 ),
 ( #13825, #13582, #12 ),
 ( #4034, #9557, #2337 ),
 ( #5941, #5127, #10065 ),
 ( #10730, #520, #7119 ),
 ( #8376, #12206, #2855 ),
 ( #14328, #3598, #1470 ),
 ( #11245, #11009, #7641 ),
 ( #4771, #1532, #8809 ),
 ( #3889, #11166, #290 ),
 ( #457, #7546, #14779 ),
 ( #13161, #5269, #365 ),
 ( #12432, #3525, #5040 ),
 ( #2636, #8295, #7408 ),
 ( #11918, #9932, #13070 ),
 ( #1186, #6220, #9841 ),
 ( #14621, #8670, #14711 ),
 ( #13448, #2715, #5203 ),
 ( #13514, #7485, #12340 ),
 ( #12273, #6284, #11077 ),
 ( #3971, #8744, #2776 ),
 ( #1612, #6376, #9998 ),
 ( #1697, #6459, #8026 ),
 ( #5349, #12664, #15016 ),
 ( #11309, #5511, #4112 ),
 ( #11488, #13758, #4336 ),
 ( #3022, #1927, #5669 ),
 ( #12509, #14848, #591 ),
 ( #10297, #13991, #682 ),
 ( #8986, #10154, #4263 ),
 ( #5440, #10234, #11404 ),
 ( #15079, #6689, #3094 ),
 ( #7787, #6522, #14941 ),
 ( #9053, #4196, #5583 ) ),
 .UNSPECIFIED., .F., .F., .T. ) 
 B_SPLINE_SURFACE_WITH_KNOTS ( ( 4, 2, 2, 2, 2, 2, 2, 2, 2, 2, 2, 2, 2, 2, 2, 2, 2, 2, 2, 2, 2, 2, 4 ),
 ( 3, 3 ),
 ( 0.000000000000000000, 0.0008763647898916152512, 0.001314547184837422823, 0.001752729579783230502, 0.002629094369674845645, 0.003505459159566461005, 0.004381823949458076364, 0.004820006344403883827, 0.005258188739349691290, 0.005696371134295498753, 0.006134553529241306216, 0.007010918319132922009, 0.007449100714078730340, 0.007887283109024537803, 0.008325465503970345266, 0.008763647898916152729, 0.009640012688807767655, 0.01051637747869938258, 0.01139274226859099751, 0.01226910705848261243, 0.01270728945342841990, 0.01314547184837422736, 0.01402183663826584402 ),
 ( 0.000000000000000000, 1.000000000000000000 ),
 .UNSPECIFIED. ) 
 GEOMETRIC_REPRESENTATION_ITEM ( )  RATIONAL_B_SPLINE_SURFACE ( (
 ( 1.000000000000000000, 0.6921057963906867005, 1.000000000000000000),
 ( 1.000000000000000000, 0.7001301295292068350, 1.000000000000000000),
 ( 1.000000000000000000, 0.7082232347829966468, 1.000000000000000000),
 ( 1.000000000000000000, 0.7204448971599605178, 1.000000000000000000),
 ( 1.000000000000000000, 0.7245324354207898221, 1.000000000000000000),
 ( 1.000000000000000000, 0.7327308554584663902, 1.000000000000000000),
 ( 1.000000000000000000, 0.7368541771550430886, 1.000000000000000000),
 ( 1.000000000000000000, 0.7489861883972682710, 1.000000000000000000),
 ( 1.000000000000000000, 0.7568423250379210376, 1.000000000000000000),
 ( 1.000000000000000000, 0.7720372848817829148, 1.000000000000000000),
 ( 1.000000000000000000, 0.7794153764102734749, 1.000000000000000000),
 ( 1.000000000000000000, 0.7929014218043154427, 1.000000000000000000),
 ( 1.000000000000000000, 0.7990977153083722584, 1.000000000000000000),
 ( 1.000000000000000000, 0.8074742350527349677, 1.000000000000000000),
 ( 1.000000000000000000, 0.8101059552811848974, 1.000000000000000000),
 ( 1.000000000000000000, 0.8149080692666150760, 1.000000000000000000),
 ( 1.000000000000000000, 0.8170977687249663113, 1.000000000000000000),
 ( 1.000000000000000000, 0.8210473395081507864, 1.000000000000000000),
 ( 1.000000000000000000, 0.8228072785942259770, 1.000000000000000000),
 ( 1.000000000000000000, 0.8258753710949300331, 1.000000000000000000),
 ( 1.000000000000000000, 0.8271879151802322694, 1.000000000000000000),
 ( 1.000000000000000000, 0.8303186452218207503, 1.000000000000000000),
 ( 1.000000000000000000, 0.8313781188583296844, 1.000000000000000000),
 ( 1.000000000000000000, 0.8314027137259931699, 1.000000000000000000),
 ( 1.000000000000000000, 0.8311425143793390591, 1.000000000000000000),
 ( 1.000000000000000000, 0.8301013997591458748, 1.000000000000000000),
 ( 1.000000000000000000, 0.8293235644851727484, 1.000000000000000000),
 ( 1.000000000000000000, 0.8272694230054146169, 1.000000000000000000),
 ( 1.000000000000000000, 0.8259930828080271903, 1.000000000000000000),
 ( 1.000000000000000000, 0.8229409194359517121, 1.000000000000000000),
 ( 1.000000000000000000, 0.8211588682283366136, 1.000000000000000000),
 ( 1.000000000000000000, 0.8152102375193999162, 1.000000000000000000),
 ( 1.000000000000000000, 0.8104135904785896294, 1.000000000000000000),
 ( 1.000000000000000000, 0.7992487876031277860, 1.000000000000000000),
 ( 1.000000000000000000, 0.7929817278871067465, 1.000000000000000000),
 ( 1.000000000000000000, 0.7794714393159598576, 1.000000000000000000),
 ( 1.000000000000000000, 0.7721045825237821125, 1.000000000000000000),
 ( 1.000000000000000000, 0.7568758627708697118, 1.000000000000000000),
 ( 1.000000000000000000, 0.7490040357394209813, 1.000000000000000000),
 ( 1.000000000000000000, 0.7368512664891039288, 1.000000000000000000),
 ( 1.000000000000000000, 0.7327258982120725683, 1.000000000000000000),
 ( 1.000000000000000000, 0.7245321423272259587, 1.000000000000000000),
 ( 1.000000000000000000, 0.7204462382506620077, 1.000000000000000000),
 ( 1.000000000000000000, 0.7082274559817631765, 1.000000000000000000),
 ( 1.000000000000000000, 0.7001335831284237754, 1.000000000000000000),
 ( 1.000000000000000000, 0.6921057963906867005, 1.000000000000000000) ) ) 
 REPRESENTATION_ITEM ( '' )  SURFACE ( )  );
#7381 = VERTEX_POINT ( 'NONE', #9285 ) ;
#7382 = ORIENTED_EDGE ( 'NONE', *, *, #8331, .F. ) ;
#7383 = AXIS2_PLACEMENT_3D ( 'NONE', #480, #13614, #2884 ) ;
#7384 = VERTEX_POINT ( 'NONE', #3255 ) ;
#7385 = CYLINDRICAL_SURFACE ( 'NONE', #11148, 0.003937007874015759253 ) ;
#7386 = CYLINDRICAL_SURFACE ( 'NONE', #8655, 0.003937007874015750579 ) ;
#7387 = EDGE_CURVE ( 'NONE', #10241, #14099, #9134, .T. ) ;
#7388 = CARTESIAN_POINT ( 'NONE',  ( 0.1062992125984795755, -0.1023622047244094474, -0.2482618547481154070 ) ) ;
#7389 = CARTESIAN_POINT ( 'NONE',  ( 0.000000000000000000, 0.007874015748031480341, 0.000000000000000000 ) ) ;
#7390 = DIRECTION ( 'NONE',  ( -0.7118260687460292724, 0.5695655044020487834, -0.4109729724067175960 ) ) ;
#7391 = AXIS2_PLACEMENT_3D ( 'NONE', #14948, #11559, #11315 ) ;
#7392 = CARTESIAN_POINT ( 'NONE',  ( -0.03886060139087894189, 0.06736074103232447818, -0.08219815605944147396 ) ) ;
#7393 = ADVANCED_FACE ( 'NONE', ( #10379 ), #909, .F. ) ;
#7394 = CARTESIAN_POINT ( 'NONE',  ( -2.183651372152203507, -1.661851685721189353, 0.08366141732283367827 ) ) ;
#7395 = AXIS2_PLACEMENT_3D ( 'NONE', #4405, #14115, #2284 ) ;
#7396 = CARTESIAN_POINT ( 'NONE',  ( 0.1023622047244639177, -0.2952755905511811330, -0.4624047872104674606 ) ) ;
#7397 = FACE_OUTER_BOUND ( 'NONE', #15158, .T. ) ;
#7398 = DIRECTION ( 'NONE',  ( -6.505213034913065258E-15, 0.000000000000000000, -1.000000000000000000 ) ) ;
#7399 = AXIS2_PLACEMENT_3D ( 'NONE', #7246, #14533, #6275 ) ;
#7400 = EDGE_CURVE ( 'NONE', #6320, #9296, #9214, .T. ) ;
#7401 = LINE ( 'NONE', #13505, #184 ) ;
#7402 = ORIENTED_EDGE ( 'NONE', *, *, #6229, .F. ) ;
#7403 = CIRCLE ( 'NONE', #14841, 0.003937007874015754916 ) ;
#7404 = ORIENTED_EDGE ( 'NONE', *, *, #5600, .F. ) ;
#7405 = AXIS2_PLACEMENT_3D ( 'NONE', #3735, #3877, #11157 ) ;
#7406 = VECTOR ( 'NONE', #669, 39.37007874015748143 ) ;
#7407 = DIRECTION ( 'NONE',  ( 0.000000000000000000, 0.000000000000000000, -1.000000000000000000 ) ) ;
#7408 = CARTESIAN_POINT ( 'NONE',  ( -1.943857306512870142, -2.935761365336657214, 0.02290380726543173040 ) ) ;
#7409 = CARTESIAN_POINT ( 'NONE',  ( -0.5615510810874360104, -0.1023622047244094474, 0.2014679098129269763 ) ) ;
#7410 = EDGE_CURVE ( 'NONE', #748, #14826, #13858, .T. ) ;
#7411 = DIRECTION ( 'NONE',  ( -1.000000000000000000, -0.000000000000000000, 0.000000000000000000 ) ) ;
#7412 = CYLINDRICAL_SURFACE ( 'NONE', #7143, 0.003937007874015749712 ) ;
#7413 = DIRECTION ( 'NONE',  ( 1.000000000000000000, 0.000000000000000000, 0.000000000000000000 ) ) ;
#7414 = CARTESIAN_POINT ( 'NONE',  ( 0.05905511811023622659, 1.338582677165354395, -0.8267716535433070613 ) ) ;
#7415 = DIRECTION ( 'NONE',  ( -0.000000000000000000, -1.000000000000000000, -0.000000000000000000 ) ) ;
#7416 = EDGE_CURVE ( 'NONE', #4753, #3491, #816, .T. ) ;
#7417 = DIRECTION ( 'NONE',  ( 0.000000000000000000, 0.000000000000000000, 1.000000000000000000 ) ) ;
#7418 = CARTESIAN_POINT ( 'NONE',  ( 0.7052242655755273093, -1.858423098537180129, 0.08366141732283417787 ) ) ;
#7419 = PRODUCT_DEFINITION_SHAPE ( 'NONE', 'NONE',  #3539 ) ;
#7420 = AXIS2_PLACEMENT_3D ( 'NONE', #1974, #788, #13872 ) ;
#7421 = VERTEX_POINT ( 'NONE', #12808 ) ;
#7422 = ORIENTED_EDGE ( 'NONE', *, *, #14781, .T. ) ;
#7423 = EDGE_LOOP ( 'NONE', ( #11184, #1419, #8142, #10736 ) ) ;
#7424 = ORIENTED_EDGE ( 'NONE', *, *, #2458, .F. ) ;
#7425 = EDGE_CURVE ( 'NONE', #984, #253, #13603, .T. ) ;
#7426 = ORIENTED_EDGE ( 'NONE', *, *, #12561, .F. ) ;
#7427 = DIRECTION ( 'NONE',  ( 0.8144815189573203495, -0.5801894994542524664, 0.000000000000000000 ) ) ;
#7428 = AXIS2_PLACEMENT_3D ( 'NONE', #12131, #155, #10864 ) ;
#7429 = PRODUCT_DEFINITION_SHAPE ( 'NONE', 'NONE',  #15478 ) ;
#7430 = PLANE ( 'NONE',  #13121 ) ;
#7431 = CARTESIAN_POINT ( 'NONE',  ( -0.1618514667033796040, -0.4921259842519685179, 0.2122517380126066888 ) ) ;
#7432 = CARTESIAN_POINT ( 'NONE',  ( -2.188531697382432029, -1.824100413744500049, 0.08366141732873445813 ) ) ;
#7433 = CARTESIAN_POINT ( 'NONE',  ( -0.09842519685028337795, -0.2952755905511811330, -0.3757906139821208802 ) ) ;
#7434 = CARTESIAN_POINT ( 'NONE',  ( -1.884762920069399161, -2.909869073764713487, 0.06183202482754375506 ) ) ;
#7435 = ORIENTED_EDGE ( 'NONE', *, *, #2152, .F. ) ;
#7436 = CARTESIAN_POINT ( 'NONE',  ( -1.972696907342682326, -2.863522232956755786, 0.1335784024945382287 ) ) ;
#7437 = FACE_OUTER_BOUND ( 'NONE', #6296, .T. ) ;
#7438 = ADVANCED_FACE ( 'NONE', ( #14063 ), #3093, .F. ) ;
#7439 = AXIS2_PLACEMENT_3D ( 'NONE', #7972, #9069, #5459 ) ;
#7440 = CARTESIAN_POINT ( 'NONE',  ( 0.06692913385832212347, -0.1023622047244094474, -0.5870514566507987197 ) ) ;
#7441 = EDGE_LOOP ( 'NONE', ( #10563, #9485, #3013, #6343 ) ) ;
#7442 = EDGE_LOOP ( 'NONE', ( #7218, #10308, #15023, #13265 ) ) ;
#7443 = AXIS2_PLACEMENT_3D ( 'NONE', #6114, #2595, #8719 ) ;
#7444 = EDGE_CURVE ( 'NONE', #11304, #2312, #14614, .T. ) ;
#7445 = ADVANCED_FACE ( 'NONE', ( #4501 ), #7846, .T. ) ;
#7446 = ORIENTED_EDGE ( 'NONE', *, *, #8742, .T. ) ;
#7447 = LINE ( 'NONE', #12244, #10634 ) ;
#7448 = CIRCLE ( 'NONE', #712, 0.003937007874015749712 ) ;
#7449 = DIRECTION ( 'NONE',  ( -0.5000000000000039968, 0.000000000000000000, -0.8660254037844362651 ) ) ;
#7450 = CARTESIAN_POINT ( 'NONE',  ( -1.293236445124221312, 0.1355266887446167634, -0.03937007874015747977 ) ) ;
#7451 = CIRCLE ( 'NONE', #3963, 0.003937007874015724558 ) ;
#7452 = FACE_OUTER_BOUND ( 'NONE', #13782, .T. ) ;
#7453 = CARTESIAN_POINT ( 'NONE',  ( -0.01755170026722350021, -0.1621998028774611911, -0.03064271692327978289 ) ) ;
#7454 = EDGE_LOOP ( 'NONE', ( #14178, #8124, #13786, #7820 ) ) ;
#7455 = CYLINDRICAL_SURFACE ( 'NONE', #10922, 0.003937007874015724558 ) ;
#7456 = CARTESIAN_POINT ( 'NONE',  ( -0.06692913385815735250, -0.4881889763779528324, -0.5909884645248143498 ) ) ;
#7457 = DIRECTION ( 'NONE',  ( -1.000000000000000000, 0.000000000000000000, 0.000000000000000000 ) ) ;
#7458 = DIRECTION ( 'NONE',  ( 0.000000000000000000, 0.000000000000000000, 1.000000000000000000 ) ) ;
#7459 = AXIS2_PLACEMENT_3D ( 'NONE', #3288, #11358, #8059 ) ;
#7460 = ORIENTED_EDGE ( 'NONE', *, *, #12303, .T. ) ;
#7461 = B_SPLINE_CURVE_WITH_KNOTS ( 'NONE', 3,
 ( #11689, #2344, #14336, #10738, #4542, #15283 ),
 .UNSPECIFIED., .F., .F.,
 ( 4, 2, 4 ),
 ( -2.828444569873699336E-06, 0.0001777364543001156273, 0.0003583013531701049201 ),
 .UNSPECIFIED. ) ;
#7462 = VERTEX_POINT ( 'NONE', #11727 ) ;
#7463 = EDGE_LOOP ( 'NONE', ( #12446, #515, #3032, #4308 ) ) ;
#7464 =( GEOMETRIC_REPRESENTATION_CONTEXT ( 3 ) GLOBAL_UNCERTAINTY_ASSIGNED_CONTEXT ( ( #13633 ) ) GLOBAL_UNIT_ASSIGNED_CONTEXT ( ( #7788, #14849, #13684 ) ) REPRESENTATION_CONTEXT ( 'NONE', 'WORKASPACE' ) );
#7465 = ORIENTED_EDGE ( 'NONE', *, *, #14916, .F. ) ;
#7466 = FACE_OUTER_BOUND ( 'NONE', #3354, .T. ) ;
#7467 = DIRECTION ( 'NONE',  ( 1.000000000000000000, 0.000000000000000000, 1.445602896647339903E-16 ) ) ;
#7468 = CARTESIAN_POINT ( 'NONE',  ( -2.116007383176099044, -1.821120273082415641, 0.1033464566929129524 ) ) ;
#7469 = LINE ( 'NONE', #6353, #4349 ) ;
#7470 = DIRECTION ( 'NONE',  ( -0.7497915094135899627, 0.5004167495348751382, -0.4328923297960366456 ) ) ;
#7471 = CARTESIAN_POINT ( 'NONE',  ( -1.574484809660005480, 0.1100025355994808662, -0.06175692796176408816 ) ) ;
#7472 = DIRECTION ( 'NONE',  ( 0.000000000000000000, 0.000000000000000000, -1.000000000000000000 ) ) ;
#7473 = DIRECTION ( 'NONE',  ( 0.5000000000000001110, 0.000000000000000000, -0.8660254037844385966 ) ) ;
#7474 = DIRECTION ( 'NONE',  ( 1.000000000000000000, 0.000000000000000000, 0.000000000000000000 ) ) ;
#7475 = CARTESIAN_POINT ( 'NONE',  ( 1.220472440944881720, 4.092325622859527280E-16, 0.02559055118110236185 ) ) ;
#7476 =( BOUNDED_SURFACE ( )  B_SPLINE_SURFACE ( 3, 2, ( 
 ( #8914, #9145, #2005 ),
 ( #15083, #5517, #13766 ),
 ( #3030, #10240, #5592 ),
 ( #11493, #12671, #6613 ),
 ( #3105, #4347, #12749 ),
 ( #602, #12583, #1850 ),
 ( #7729, #1776, #11318 ),
 ( #3189, #6771, #1935 ),
 ( #11561, #7796, #10072 ),
 ( #10392, #4273, #4437 ) ),
 .UNSPECIFIED., .F., .F., .T. ) 
 B_SPLINE_SURFACE_WITH_KNOTS ( ( 4, 2, 2, 2, 4 ),
 ( 3, 3 ),
 ( -1.040834085586084257E-17, 0.01438982281936204699, 0.02158473422904307742, 0.02518218993388358917, 0.02877964563872410439 ),
 ( 0.000000000000000000, 1.000000000000000000 ),
 .UNSPECIFIED. ) 
 GEOMETRIC_REPRESENTATION_ITEM ( )  RATIONAL_B_SPLINE_SURFACE ( (
 ( 1.000000000000000000, 0.7214151048183972126, 1.000000000000000000),
 ( 1.000000000000000000, 0.7162796536165754180, 1.000000000000000000),
 ( 1.000000000000000000, 0.7123718545348233233, 1.000000000000000000),
 ( 1.000000000000000000, 0.7086903259631885943, 1.000000000000000000),
 ( 1.000000000000000000, 0.7078262380797001319, 1.000000000000000000),
 ( 1.000000000000000000, 0.7071130014577271528, 1.000000000000000000),
 ( 1.000000000000000000, 0.7069727248725110602, 1.000000000000000000),
 ( 1.000000000000000000, 0.7068914992104640138, 1.000000000000000000),
 ( 1.000000000000000000, 0.7069499230734396233, 1.000000000000000000),
 ( 1.000000000000000000, 0.7071067811865475727, 1.000000000000000000) ) ) 
 REPRESENTATION_ITEM ( '' )  SURFACE ( )  );
#7477 = DIRECTION ( 'NONE',  ( -1.000000000000000000, -0.000000000000000000, -3.476578583725179813E-16 ) ) ;
#7478 = ORIENTED_EDGE ( 'NONE', *, *, #513, .F. ) ;
#7479 = ADVANCED_FACE ( 'NONE', ( #278 ), #1365, .T. ) ;
#7480 = ORIENTED_EDGE ( 'NONE', *, *, #7410, .T. ) ;
#7481 = ADVANCED_FACE ( 'NONE', ( #14529 ), #9590, .T. ) ;
#7482 = VERTEX_POINT ( 'NONE', #2531 ) ;
#7483 = EDGE_CURVE ( 'NONE', #14569, #13096, #4103, .T. ) ;
#7484 = CARTESIAN_POINT ( 'NONE',  ( -0.3964138223131424832, -0.2952755905511811330, 0.1515865201236451798 ) ) ;
#7485 = CARTESIAN_POINT ( 'NONE',  ( -1.943645325779189470, -2.936341075933833977, 0.06731275603298569887 ) ) ;
#7486 = DIRECTION ( 'NONE',  ( -0.03006568382583901106, -0.9995479251422039191, 0.000000000000000000 ) ) ;
#7487 = CARTESIAN_POINT ( 'NONE',  ( 0.5084014747882494856, -0.4881889763779528324, 0.2935257283254013583 ) ) ;
#7488 = DIRECTION ( 'NONE',  ( 0.5000000000000004441, 0.000000000000000000, -0.8660254037844382635 ) ) ;
#7489 = DIRECTION ( 'NONE',  ( 1.000000000000000000, 0.000000000000000000, 0.000000000000000000 ) ) ;
#7490 = LINE ( 'NONE', #5134, #906 ) ;
#7491 = CARTESIAN_POINT ( 'NONE',  ( -1.887573697862731770, -2.902928153145550638, -0.07679814701984788439 ) ) ;
#7492 = LINE ( 'NONE', #297, #2822 ) ;
#7493 = FACE_OUTER_BOUND ( 'NONE', #12181, .T. ) ;
#7494 = ORIENTED_EDGE ( 'NONE', *, *, #13482, .F. ) ;
#7495 = EDGE_CURVE ( 'NONE', #315, #12429, #10698, .T. ) ;
#7496 = ORIENTED_EDGE ( 'NONE', *, *, #12584, .F. ) ;
#7497 = EDGE_LOOP ( 'NONE', ( #6537, #8872, #2687, #5392 ) ) ;
#7498 = EDGE_CURVE ( 'NONE', #13738, #924, #12612, .T. ) ;
#7499 = ORIENTED_EDGE ( 'NONE', *, *, #6726, .T. ) ;
#7500 =( REPRESENTATION_RELATIONSHIP ('NONE','NONE', #8904, #12105 ) REPRESENTATION_RELATIONSHIP_WITH_TRANSFORMATION ( #10681 )SHAPE_REPRESENTATION_RELATIONSHIP( ) );
#7501 = EDGE_LOOP ( 'NONE', ( #14309, #7193, #9335 ) ) ;
#7502 = DIRECTION ( 'NONE',  ( 0.4999999999999979461, -0.000000000000000000, 0.8660254037844398178 ) ) ;
#7503 = EDGE_CURVE ( 'NONE', #9212, #13179, #6076, .T. ) ;
#7504 = CARTESIAN_POINT ( 'NONE',  ( -0.2393297813659119588, -0.09842519685039370636, 0.06089400679736759608 ) ) ;
#7505 = DIRECTION ( 'NONE',  ( -1.000000000000000000, -0.000000000000000000, 0.000000000000000000 ) ) ;
#7506 = DIRECTION ( 'NONE',  ( 0.5801894994542512451, 0.8144815189573213488, 0.000000000000000000 ) ) ;
#7507 = CARTESIAN_POINT ( 'NONE',  ( -1.992382107315058271, -2.749515453455440905, 0.1756903148397124803 ) ) ;
#7508 = DIRECTION ( 'NONE',  ( 0.000000000000000000, 0.000000000000000000, 1.000000000000000000 ) ) ;
#7509 = CARTESIAN_POINT ( 'NONE',  ( -1.898906488563334882, -2.946676766132140468, -0.03212724755967235474 ) ) ;
#7510 = ORIENTED_EDGE ( 'NONE', *, *, #3126, .F. ) ;
#7511 = CARTESIAN_POINT ( 'NONE',  ( -1.419615703680148000, -0.01226548409420232313, 0.07874015748031495954 ) ) ;
#7512 = CARTESIAN_POINT ( 'NONE',  ( -1.588298999900524366, 0.1240273096569512873, 0.05983744915181773982 ) ) ;
#7513 = CARTESIAN_POINT ( 'NONE',  ( -1.419024763034335335, -0.01190114260487083048, -0.07304054665220574560 ) ) ;
#7514 = ORIENTED_EDGE ( 'NONE', *, *, #9712, .F. ) ;
#7515 = ORIENTED_EDGE ( 'NONE', *, *, #2244, .T. ) ;
#7516 = ORIENTED_EDGE ( 'NONE', *, *, #11462, .T. ) ;
#7517 = EDGE_CURVE ( 'NONE', #6904, #5548, #9107, .T. ) ;
#7518 = EDGE_CURVE ( 'NONE', #4513, #8855, #9526, .T. ) ;
#7519 = DIRECTION ( 'NONE',  ( 0.000000000000000000, -0.000000000000000000, -1.000000000000000000 ) ) ;
#7520 = DIRECTION ( 'NONE',  ( -0.4999999999999996114, -0.000000000000000000, -0.8660254037844389297 ) ) ;
#7521 = DIRECTION ( 'NONE',  ( 1.000000000000000000, 0.000000000000000000, -1.224646799147353207E-16 ) ) ;
#7522 = CARTESIAN_POINT ( 'NONE',  ( -0.6692913385826770867, 1.614173228346457156, 0.000000000000000000 ) ) ;
#7523 = ORIENTED_EDGE ( 'NONE', *, *, #5135, .T. ) ;
#7524 = DIRECTION ( 'NONE',  ( 0.4999999999999918954, -0.000000000000000000, -0.8660254037844431485 ) ) ;
#7525 = EDGE_CURVE ( 'NONE', #7766, #10116, #1108, .T. ) ;
#7526 = CARTESIAN_POINT ( 'NONE',  ( 0.06299212598430636856, -0.2952755905511811330, -0.4190977005962941426 ) ) ;
#7527 = CARTESIAN_POINT ( 'NONE',  ( 0.5413385826771386355, -0.1023622047244094474, 0.2443509997554994817 ) ) ;
#7528 = FILL_AREA_STYLE ('',( #11221 ) ) ;
#7529 = ORIENTED_EDGE ( 'NONE', *, *, #2157, .F. ) ;
#7530 = ORIENTED_EDGE ( 'NONE', *, *, #3001, .T. ) ;
#7531 = DIRECTION ( 'NONE',  ( 0.000000000000000000, -1.000000000000000000, 0.000000000000000000 ) ) ;
#7532 = CARTESIAN_POINT ( 'NONE',  ( 0.000000000000000000, 2.393700787401575436, 0.5433070866141731514 ) ) ;
#7533 = CARTESIAN_POINT ( 'NONE',  ( -2.011286886001135255, -2.518997274786896945, 0.1294465814784910018 ) ) ;
#7534 = DIRECTION ( 'NONE',  ( 0.000000000000000000, 0.000000000000000000, 1.000000000000000000 ) ) ;
#7535 = CARTESIAN_POINT ( 'NONE',  ( -0.08858267716538309466, 36.23251143493367721, -1.111019662821376208 ) ) ;
#7536 = DIRECTION ( 'NONE',  ( 0.000000000000000000, 0.000000000000000000, 1.000000000000000000 ) ) ;
#7537 = CARTESIAN_POINT ( 'NONE',  ( -1.293236445124221312, 0.1355266887446167634, 0.03937007874015747977 ) ) ;
#7538 = EDGE_CURVE ( 'NONE', #241, #7384, #2301, .T. ) ;
#7539 = LINE ( 'NONE', #11390, #10131 ) ;
#7540 = DIRECTION ( 'NONE',  ( 0.000000000000000000, -1.000000000000000000, -0.000000000000000000 ) ) ;
#7541 = ORIENTED_EDGE ( 'NONE', *, *, #11825, .F. ) ;
#7542 = ORIENTED_EDGE ( 'NONE', *, *, #747, .T. ) ;
#7543 = EDGE_LOOP ( 'NONE', ( #7303, #10395, #13424, #8293 ) ) ;
#7544 = ORIENTED_EDGE ( 'NONE', *, *, #5501, .T. ) ;
#7545 = CARTESIAN_POINT ( 'NONE',  ( 0.2652685895082805834, -0.4921259842519685179, 0.03495519865525829883 ) ) ;
#7546 = CARTESIAN_POINT ( 'NONE',  ( -1.938182383310145918, -2.949473540663261950, -0.01292403952254523800 ) ) ;
#7547 = CARTESIAN_POINT ( 'NONE',  ( 0.000000000000000000, 0.000000000000000000, 0.000000000000000000 ) ) ;
#7548 = DIRECTION ( 'NONE',  ( 1.000000000000000000, 0.000000000000000000, -1.224646799147353207E-16 ) ) ;
#7549 = CARTESIAN_POINT ( 'NONE',  ( -2.007193303979263543, -2.769482957687897873, -0.1575906666632094777 ) ) ;
#7550 = CARTESIAN_POINT ( 'NONE',  ( -1.181102362204724310, -0.1279527559055117225, -0.02559055118110236185 ) ) ;
#7551 = CARTESIAN_POINT ( 'NONE',  ( 0.000000000000000000, 2.637795275590551825, 0.03937007874015747977 ) ) ;
#7552 = EDGE_CURVE ( 'NONE', #15252, #6320, #3100, .T. ) ;
#7553 = FACE_OUTER_BOUND ( 'NONE', #2649, .T. ) ;
#7554 = FACE_OUTER_BOUND ( 'NONE', #3778, .T. ) ;
#7555 = DIRECTION ( 'NONE',  ( 0.000000000000000000, 1.000000000000000000, 0.000000000000000000 ) ) ;
#7556 = ORIENTED_EDGE ( 'NONE', *, *, #11600, .T. ) ;
#7557 = ADVANCED_FACE ( 'NONE', ( #6126 ), #8860, .F. ) ;
#7558 = ORIENTED_EDGE ( 'NONE', *, *, #422, .T. ) ;
#7559 = ORIENTED_EDGE ( 'NONE', *, *, #8727, .F. ) ;
#7560 = EDGE_LOOP ( 'NONE', ( #5901, #5265, #11160, #254 ) ) ;
#7561 = EDGE_LOOP ( 'NONE', ( #8228, #7688, #14012, #8188 ) ) ;
#7562 = CARTESIAN_POINT ( 'NONE',  ( -1.417802900492933782, -0.04287136159519128187, -0.07874015748031495954 ) ) ;
#7563 = DIRECTION ( 'NONE',  ( -0.000000000000000000, -1.000000000000000000, -0.000000000000000000 ) ) ;
#7564 = TOROIDAL_SURFACE ( 'NONE', #9846, 0.007874015748031495954, 0.003937007874015747977 ) ;
#7565 = AXIS2_PLACEMENT_3D ( 'NONE', #14248, #2096, #8283 ) ;
#7566 = CARTESIAN_POINT ( 'NONE',  ( -1.181102362204724310, 0.000000000000000000, 0.02952755905511811330 ) ) ;
#7567 = FACE_OUTER_BOUND ( 'NONE', #7698, .T. ) ;
#7568 = VECTOR ( 'NONE', #4283, 39.37007874015748143 ) ;
#7569 = CYLINDRICAL_SURFACE ( 'NONE', #11337, 0.003937007874015749712 ) ;
#7570 = CARTESIAN_POINT ( 'NONE',  ( -1.185456167500018365, 0.3350708678533356188, 0.05695194461341470532 ) ) ;
#7571 = CARTESIAN_POINT ( 'NONE',  ( -1.869830193481172520, -2.946302503418662511, -0.03424462898272506023 ) ) ;
#7572 = ADVANCED_FACE ( 'NONE', ( #10830 ), #3644, .F. ) ;
#7573 = ORIENTED_EDGE ( 'NONE', *, *, #2408, .T. ) ;
#7574 = CARTESIAN_POINT ( 'NONE',  ( -1.224409448818897461, 5.303588500244450842E-18, -0.02559055118110236185 ) ) ;
#7575 = FACE_OUTER_BOUND ( 'NONE', #7543, .T. ) ;
#7576 = DIRECTION ( 'NONE',  ( 0.000000000000000000, 0.000000000000000000, -1.000000000000000000 ) ) ;
#7578 = EDGE_LOOP ( 'NONE', ( #6230, #2946, #13246, #32 ) ) ;
#7577 = APPLICATION_CONTEXT ( 'automotive_design' ) ;
#7579 = EDGE_CURVE ( 'NONE', #2898, #12827, #11963, .T. ) ;
#7580 = ORIENTED_EDGE ( 'NONE', *, *, #12425, .F. ) ;
#7581 = CIRCLE ( 'NONE', #7096, 0.03937007874015751446 ) ;
#7582 = VECTOR ( 'NONE', #2953, 39.37007874015748143 ) ;
#7583 = AXIS2_PLACEMENT_3D ( 'NONE', #6659, #13734, #6805 ) ;
#7584 = CIRCLE ( 'NONE', #11603, 0.05905511811023627516 ) ;
#7585 = ORIENTED_EDGE ( 'NONE', *, *, #5790, .T. ) ;
#7586 = EDGE_CURVE ( 'NONE', #115, #7799, #1602, .T. ) ;
#7587 = DIRECTION ( 'NONE',  ( -0.000000000000000000, -1.000000000000000000, -0.000000000000000000 ) ) ;
#7588 = CARTESIAN_POINT ( 'NONE',  ( -0.1586168312385622392, -0.09448818897637796532, -0.5890199605878065903 ) ) ;
#7589 = TOROIDAL_SURFACE ( 'NONE', #852, 0.04330708661417328326, 0.003937007874015747977 ) ;
#7590 = CARTESIAN_POINT ( 'NONE',  ( 1.181102362204724310, 0.1240157480314959815, -0.02952755905511811330 ) ) ;
#7591 = AXIS2_PLACEMENT_3D ( 'NONE', #13040, #123, #9762 ) ;
#7592 = CARTESIAN_POINT ( 'NONE',  ( -0.06145017734370220031, -0.1666692956086705812, -0.05763041683086380512 ) ) ;
#7593 = ADVANCED_FACE ( 'NONE', ( #8421 ), #2469, .T. ) ;
#7594 = VERTEX_POINT ( 'NONE', #7306 ) ;
#7595 = DIRECTION ( 'NONE',  ( 0.000000000000000000, 0.000000000000000000, -1.000000000000000000 ) ) ;
#7596 = AXIS2_PLACEMENT_3D ( 'NONE', #9968, #8625, #10032 ) ;
#7597 = VECTOR ( 'NONE', #11835, 39.37007874015748854 ) ;
#7598 = DIRECTION ( 'NONE',  ( 1.224646799147353207E-16, 0.000000000000000000, -1.000000000000000000 ) ) ;
#7599 = AXIS2_PLACEMENT_3D ( 'NONE', #15297, #28, #10517 ) ;
#7600 = DIRECTION ( 'NONE',  ( 0.000000000000000000, 1.000000000000000000, 0.000000000000000000 ) ) ;
#7601 = CARTESIAN_POINT ( 'NONE',  ( -1.412372674844927456, -0.03807050201945849643, 0.05475977885638705356 ) ) ;
#7602 = AXIS2_PLACEMENT_3D ( 'NONE', #14231, #6272, #13208 ) ;
#7603 = EDGE_CURVE ( 'NONE', #8519, #12965, #2104, .T. ) ;
#7604 = CYLINDRICAL_SURFACE ( 'NONE', #9694, 0.1574803149606299191 ) ;
#7605 = EDGE_LOOP ( 'NONE', ( #2018, #13523, #4104, #6248 ) ) ;
#7607 = ORIENTED_EDGE ( 'NONE', *, *, #5506, .T. ) ;
#7606 = AXIS2_PLACEMENT_3D ( 'NONE', #11474, #742, #8544 ) ;
#7608 = CIRCLE ( 'NONE', #2162, 0.03937007874015747977 ) ;
#7609 = CIRCLE ( 'NONE', #12376, 0.01968503937007880233 ) ;
#7610 = ORIENTED_EDGE ( 'NONE', *, *, #9137, .F. ) ;
#7611 = AXIS2_PLACEMENT_3D ( 'NONE', #3134, #2109, #10327 ) ;
#7612 = AXIS2_PLACEMENT_3D ( 'NONE', #1256, #9641, #8150 ) ;
#7613 = ADVANCED_FACE ( 'NONE', ( #2696 ), #7984, .T. ) ;
#7614 = DIRECTION ( 'NONE',  ( -0.000000000000000000, -1.000000000000000000, -0.000000000000000000 ) ) ;
#7615 = DIRECTION ( 'NONE',  ( 1.000000000000000000, 0.000000000000000000, -1.669238443041289155E-16 ) ) ;
#7616 = AXIS2_PLACEMENT_3D ( 'NONE', #9744, #4948, #9969 ) ;
#7617 = CARTESIAN_POINT ( 'NONE',  ( -1.107198012490790529, -0.06846922848666055217, -0.03937007874015747977 ) ) ;
#7618 = DIRECTION ( 'NONE',  ( 0.000000000000000000, 0.000000000000000000, 1.000000000000000000 ) ) ;
#7619 = CARTESIAN_POINT ( 'NONE',  ( 0.9178799135247481811, 36.23251143493369142, 0.6322246801711491893 ) ) ;
#7620 = DIRECTION ( 'NONE',  ( 1.000000000000000000, -0.000000000000000000, -0.000000000000000000 ) ) ;
#7621 = DIRECTION ( 'NONE',  ( -0.000000000000000000, -0.000000000000000000, -1.000000000000000000 ) ) ;
#7622 = DIRECTION ( 'NONE',  ( 0.000000000000000000, 0.000000000000000000, -1.000000000000000000 ) ) ;
#7623 = CARTESIAN_POINT ( 'NONE',  ( -0.1724006475077544398, -0.1023622047244094474, 0.1728816592724491952 ) ) ;
#7624 = DIRECTION ( 'NONE',  ( 0.000000000000000000, -1.000000000000000000, -0.000000000000000000 ) ) ;
#7625 = CIRCLE ( 'NONE', #14393, 0.7086614173228346081 ) ;
#7626 = AXIS2_PLACEMENT_3D ( 'NONE', #7065, #14052, #11714 ) ;
#7627 = AXIS2_PLACEMENT_3D ( 'NONE', #2732, #7502, #9950 ) ;
#7628 = DIRECTION ( 'NONE',  ( 0.3235667741753642801, -0.9383274424966858707, 0.1218447918762963489 ) ) ;
#7629 = ADVANCED_FACE ( 'NONE', ( #2836 ), #12558, .F. ) ;
#7630 = ORIENTED_EDGE ( 'NONE', *, *, #15456, .F. ) ;
#7631 = CIRCLE ( 'NONE', #10649, 0.003937007874015724558 ) ;
#7632 = ORIENTED_EDGE ( 'NONE', *, *, #13508, .F. ) ;
#7633 = LINE ( 'NONE', #581, #7361 ) ;
#7634 = VERTEX_POINT ( 'NONE', #5329 ) ;
#7635 = VERTEX_POINT ( 'NONE', #7617 ) ;
#7636 = ADVANCED_FACE ( 'NONE', ( #6506 ), #5108, .T. ) ;
#7637 = TOROIDAL_SURFACE ( 'NONE', #12401, 0.007874015748031495954, 0.003937007874015747977 ) ;
#7638 = VECTOR ( 'NONE', #13228, 39.37007874015748143 ) ;
#7639 = AXIS2_PLACEMENT_3D ( 'NONE', #3721, #8496, #13269 ) ;
#7640 = PLANE ( 'NONE',  #14613 ) ;
#7641 = CARTESIAN_POINT ( 'NONE',  ( -1.945984862809333915, -2.930601869584705366, -0.04578774291266937690 ) ) ;
#7642 = AXIS2_PLACEMENT_3D ( 'NONE', #5586, #10386, #10540 ) ;
#7643 = B_SPLINE_CURVE_WITH_KNOTS ( 'NONE', 3,
 ( #12279, #2956, #5046, #14635, #3897, #1539, #6529, #296, #5276, #3978, #8677, #14718, #2865, #11252, #13455, #11084, #8751, #525, #374, #10366, #10070, #9940, #2723, #2642, #11316, #7491, #6290, #13690, #8912, #14855, #4121, #465, #13520, #8587, #2781, #8815, #7726, #7648 ),
 .UNSPECIFIED., .F., .F.,
 ( 4, 2, 2, 2, 2, 2, 2, 2, 2, 2, 2, 2, 2, 2, 2, 2, 2, 2, 4 ),
 ( 0.000000000000000000, 0.0008718204131946265560, 0.001743640826389253112, 0.002615461239583880427, 0.003487281652778507959, 0.004359102065973135924, 0.005230922479167762588, 0.005666832685765068114, 0.006102742892362373640, 0.006974563305556972549, 0.007410473512154272004, 0.007846383718751572325, 0.008718204131946159091, 0.009590024545140745857, 0.01046184495833533436, 0.01133366537152992286, 0.01220548578472450962, 0.01307730619791909812, 0.01394912661111368489 ),
 .UNSPECIFIED. ) ;
#7644 = CARTESIAN_POINT ( 'NONE',  ( 0.4330708661417309036, -0.09448818897637796532, 0.4318761856142889766 ) ) ;
#7645 = DIRECTION ( 'NONE',  ( 0.000000000000000000, 0.000000000000000000, 1.000000000000000000 ) ) ;
#7646 = DIRECTION ( 'NONE',  ( -0.000000000000000000, 1.000000000000000000, 0.000000000000000000 ) ) ;
#7647 = CARTESIAN_POINT ( 'NONE',  ( 0.1023622047244639455, -0.4881889763779528324, -0.5870514566507987197 ) ) ;
#7648 = CARTESIAN_POINT ( 'NONE',  ( -1.945459748359985142, -2.745801194614594820, -0.1561691687464109024 ) ) ;
#7649 = FACE_OUTER_BOUND ( 'NONE', #11822, .T. ) ;
#7650 = PLANE ( 'NONE',  #10409 ) ;
#7651 = AXIS2_PLACEMENT_3D ( 'NONE', #6959, #11752, #1015 ) ;
#7652 = AXIS2_PLACEMENT_3D ( 'NONE', #7418, #12217, #12281 ) ;
#7653 = AXIS2_PLACEMENT_3D ( 'NONE', #7971, #6708, #15093 ) ;
#7654 = ORIENTED_EDGE ( 'NONE', *, *, #7960, .F. ) ;
#7655 = ORIENTED_EDGE ( 'NONE', *, *, #7374, .F. ) ;
#7656 = ORIENTED_EDGE ( 'NONE', *, *, #15185, .F. ) ;
#7657 = CIRCLE ( 'NONE', #4153, 0.5511811023622046335 ) ;
#7658 = VERTEX_POINT ( 'NONE', #5183 ) ;
#7659 = VERTEX_POINT ( 'NONE', #10048 ) ;
#7660 = CARTESIAN_POINT ( 'NONE',  ( -1.387704745771440429, -0.02010536753476140082, -0.05905511811023623353 ) ) ;
#7661 = FACE_OUTER_BOUND ( 'NONE', #5572, .T. ) ;
#7662 = CARTESIAN_POINT ( 'NONE',  ( 0.5418660417173575272, -0.1023622047244094474, 0.2355633981508976349 ) ) ;
#7663 = CIRCLE ( 'NONE', #9927, 0.01968503937007868437 ) ;
#7664 = CARTESIAN_POINT ( 'NONE',  ( -2.184126211765464287, -1.725292181286280258, -0.08417626406393655114 ) ) ;
#7665 = DIRECTION ( 'NONE',  ( 0.000000000000000000, 0.000000000000000000, -1.000000000000000000 ) ) ;
#7666 = CARTESIAN_POINT ( 'NONE',  ( -1.220472440944881720, 0.000000000000000000, 0.02559055118110236185 ) ) ;
#7667 = DIRECTION ( 'NONE',  ( 1.000000000000000000, -8.673617379884032514E-16, 0.000000000000000000 ) ) ;
#7668 = CARTESIAN_POINT ( 'NONE',  ( 0.5068643957867006167, 1.043307086614173373, 0.2244473186741426096 ) ) ;
#7669 = AXIS2_PLACEMENT_3D ( 'NONE', #7689, #3059, #14676 ) ;
#7670 = CARTESIAN_POINT ( 'NONE',  ( -1.869182993986379326, -2.947846950676647371, 0.02785115562066423078 ) ) ;
#7671 = ORIENTED_EDGE ( 'NONE', *, *, #13005, .T. ) ;
#7672 = CARTESIAN_POINT ( 'NONE',  ( -2.188531697382454677, -1.824100413745272764, -0.08366141732860882252 ) ) ;
#7673 = CARTESIAN_POINT ( 'NONE',  ( -0.06299212598414158371, -0.2952755905511811330, -0.4624047872104674606 ) ) ;
#7674 = ORIENTED_EDGE ( 'NONE', *, *, #3893, .F. ) ;
#7675 = ORIENTED_EDGE ( 'NONE', *, *, #15195, .T. ) ;
#7676 = AXIS2_PLACEMENT_3D ( 'NONE', #5174, #6501, #13879 ) ;
#7677 = EDGE_CURVE ( 'NONE', #4061, #13962, #10854, .T. ) ;
#7678 = EDGE_LOOP ( 'NONE', ( #6906, #13699, #2232, #1486, #9230 ) ) ;
#7679 = AXIS2_PLACEMENT_3D ( 'NONE', #11576, #15193, #9240 ) ;
#7680 = ADVANCED_FACE ( 'NONE', ( #14829 ), #5865, .T. ) ;
#7681 = AXIS2_PLACEMENT_3D ( 'NONE', #10750, #7148, #9572 ) ;
#7682 = EDGE_CURVE ( 'NONE', #12044, #5876, #10101, .T. ) ;
#7683 = CARTESIAN_POINT ( 'NONE',  ( 0.000000000000000000, -0.4921259842519685179, -0.1535433070866141780 ) ) ;
#7684 = DIRECTION ( 'NONE',  ( 0.000000000000000000, 0.000000000000000000, -1.000000000000000000 ) ) ;
#7686 = AXIS2_PLACEMENT_3D ( 'NONE', #9544, #6286, #12122 ) ;
#7685 = LINE ( 'NONE', #13410, #1712 ) ;
#7687 = CARTESIAN_POINT ( 'NONE',  ( 0.000000000000000000, 1.346456692913385877, 0.000000000000000000 ) ) ;
#7688 = ORIENTED_EDGE ( 'NONE', *, *, #5653, .F. ) ;
#7689 = CARTESIAN_POINT ( 'NONE',  ( 0.000000000000000000, 0.000000000000000000, 0.000000000000000000 ) ) ;
#7690 = FACE_OUTER_BOUND ( 'NONE', #4331, .T. ) ;
#7691 = CARTESIAN_POINT ( 'NONE',  ( 0.05175539059627461136, 0.000000000000000000, -0.07475334604056278753 ) ) ;
#7692 = CIRCLE ( 'NONE', #9707, 0.007874015748031516770 ) ;
#7693 = LINE ( 'NONE', #1896, #9467 ) ;
#7694 = DIRECTION ( 'NONE',  ( 0.000000000000000000, 0.000000000000000000, -1.000000000000000000 ) ) ;
#7695 = CIRCLE ( 'NONE', #3699, 0.005905511811023620231 ) ;
#7696 = EDGE_LOOP ( 'NONE', ( #7780, #2729, #5143, #12318 ) ) ;
#7697 = ADVANCED_FACE ( 'NONE', ( #14998 ), #3069, .F. ) ;
#7698 = EDGE_LOOP ( 'NONE', ( #12765, #12632, #717, #12243 ) ) ;
#7699 = AXIS2_PLACEMENT_3D ( 'NONE', #1616, #2952, #10300 ) ;
#7700 = EDGE_CURVE ( 'NONE', #2187, #4456, #5327, .T. ) ;
#7701 = ORIENTED_EDGE ( 'NONE', *, *, #3763, .T. ) ;
#7702 = DIRECTION ( 'NONE',  ( -0.4999999999999998335, 0.000000000000000000, -0.8660254037844388186 ) ) ;
#7703 = DIRECTION ( 'NONE',  ( 0.000000000000000000, 0.000000000000000000, -1.000000000000000000 ) ) ;
#7704 = TOROIDAL_SURFACE ( 'NONE', #12468, 0.007874015748031495954, 0.003937007874015747977 ) ;
#7705 = EDGE_CURVE ( 'NONE', #13131, #5345, #12866, .T. ) ;
#7706 = DIRECTION ( 'NONE',  ( 0.000000000000000000, 2.212657494868377674E-16, -1.000000000000000000 ) ) ;
#7707 = ADVANCED_FACE ( 'NONE', ( #7848, #10216 ), #2137, .F. ) ;
#7708 = LINE ( 'NONE', #5334, #1629 ) ;
#7709 = CARTESIAN_POINT ( 'NONE',  ( 0.1062992125984795477, -0.1023622047244094474, -0.2482618547481154347 ) ) ;
#7710 = CARTESIAN_POINT ( 'NONE',  ( -0.1181102362204724532, 2.637795275590551825, -0.03937007874015747977 ) ) ;
#7711 = LINE ( 'NONE', #1597, #8382 ) ;
#7712 = AXIS2_PLACEMENT_3D ( 'NONE', #7916, #15045, #13869 ) ;
#7713 = CYLINDRICAL_SURFACE ( 'NONE', #2656, 0.1279527559055117780 ) ;
#7714 =( GEOMETRIC_REPRESENTATION_CONTEXT ( 3 ) GLOBAL_UNCERTAINTY_ASSIGNED_CONTEXT ( ( #2981 ) ) GLOBAL_UNIT_ASSIGNED_CONTEXT ( ( #15165, #994, #15246 ) ) REPRESENTATION_CONTEXT ( 'NONE', 'WORKASPACE' ) );
#7715 = ORIENTED_EDGE ( 'NONE', *, *, #6726, .F. ) ;
#7716 = CARTESIAN_POINT ( 'NONE',  ( 0.000000000000000000, 0.04724409448818898960, 0.000000000000000000 ) ) ;
#7717 = ORIENTED_EDGE ( 'NONE', *, *, #7798, .F. ) ;
#7718 = ORIENTED_EDGE ( 'NONE', *, *, #12800, .F. ) ;
#7719 = CARTESIAN_POINT ( 'NONE',  ( -0.5413385826771385245, -0.1023622047244094474, 0.2443509997554989266 ) ) ;
#7720 = DIRECTION ( 'NONE',  ( -0.8660254037844363761, 0.000000000000000000, 0.5000000000000038858 ) ) ;
#7721 = EDGE_CURVE ( 'NONE', #15201, #9446, #12790, .T. ) ;
#7722 = CARTESIAN_POINT ( 'NONE',  ( 0.000000000000000000, 1.346456692913385877, 0.000000000000000000 ) ) ;
#7723 = CARTESIAN_POINT ( 'NONE',  ( 0.5398975377803496567, -0.1023622047244094474, 0.2389729469846946508 ) ) ;
#7724 = CARTESIAN_POINT ( 'NONE',  ( 0.1586168312385622392, -0.09448818897637796532, -0.5890199605878065903 ) ) ;
#7725 = CARTESIAN_POINT ( 'NONE',  ( 0.000000000000000000, 1.043307086614173596, -3.902639990948922033E-18 ) ) ;
#7726 = CARTESIAN_POINT ( 'NONE',  ( -1.941800925136052181, -2.756730452697893963, -0.1575983618999967639 ) ) ;
#7727 = EDGE_CURVE ( 'NONE', #984, #2367, #1846, .T. ) ;
#7728 = DIRECTION ( 'NONE',  ( 0.000000000000000000, 1.000000000000000000, 0.000000000000000000 ) ) ;
#7729 = CARTESIAN_POINT ( 'NONE',  ( -2.109904382371071918, -1.821337472029024074, -0.1053091407001082030 ) ) ;
#7730 = ORIENTED_EDGE ( 'NONE', *, *, #7781, .T. ) ;
#7731 = VERTEX_POINT ( 'NONE', #11613 ) ;
#7732 = ORIENTED_EDGE ( 'NONE', *, *, #8939, .T. ) ;
#7733 = ORIENTED_EDGE ( 'NONE', *, *, #1856, .T. ) ;
#7734 = ORIENTED_EDGE ( 'NONE', *, *, #4754, .T. ) ;
#7735 = FACE_OUTER_BOUND ( 'NONE', #12591, .T. ) ;
#7736 = DIRECTION ( 'NONE',  ( 0.000000000000000000, 2.212657494868377674E-16, -1.000000000000000000 ) ) ;
#7737 = CARTESIAN_POINT ( 'NONE',  ( 0.06692913385832215123, -0.4881889763779528324, -0.5870514566507987197 ) ) ;
#7738 = LINE ( 'NONE', #8832, #14456 ) ;
#7739 = DIRECTION ( 'NONE',  ( 0.8660254037844365982, -0.000000000000000000, 0.5000000000000035527 ) ) ;
#7740 = DIRECTION ( 'NONE',  ( 1.000000000000000000, -0.000000000000000000, -0.000000000000000000 ) ) ;
#7741 = DIRECTION ( 'NONE',  ( -0.000000000000000000, -1.000000000000000000, -0.000000000000000000 ) ) ;
#7742 = DIRECTION ( 'NONE',  ( 0.000000000000000000, 0.000000000000000000, -1.000000000000000000 ) ) ;
#7743 = CARTESIAN_POINT ( 'NONE',  ( -1.898002436973827756, -2.949150955976388211, -0.01280807431238822208 ) ) ;
#7744 = VERTEX_POINT ( 'NONE', #4248 ) ;
#7745 = CARTESIAN_POINT ( 'NONE',  ( -1.276200637803905691, -0.1988000726501942539, 0.08366141732283455257 ) ) ;
#7746 = EDGE_CURVE ( 'NONE', #14569, #11092, #12728, .T. ) ;
#7747 = DIRECTION ( 'NONE',  ( 0.8660254037844365982, -0.000000000000000000, 0.5000000000000035527 ) ) ;
#7748 = ORIENTED_EDGE ( 'NONE', *, *, #2365, .F. ) ;
#7749 = EDGE_LOOP ( 'NONE', ( #518, #12676 ) ) ;
#7750 = ORIENTED_EDGE ( 'NONE', *, *, #14043, .F. ) ;
#7751 = DIRECTION ( 'NONE',  ( -0.000000000000000000, -1.000000000000000000, -0.000000000000000000 ) ) ;
#7752 = DIRECTION ( 'NONE',  ( 1.000000000000000000, 0.000000000000000000, 0.000000000000000000 ) ) ;
#7753 = CARTESIAN_POINT ( 'NONE',  ( -1.100415514366347880, -0.04998955061626794705, -0.03937007874015747977 ) ) ;
#7754 = DIRECTION ( 'NONE',  ( -1.000000000000000000, -0.000000000000000000, -0.000000000000000000 ) ) ;
#7755 = DIRECTION ( 'NONE',  ( 0.000000000000000000, 1.000000000000000000, 0.000000000000000000 ) ) ;
#7756 = ORIENTED_EDGE ( 'NONE', *, *, #2756, .T. ) ;
#7757 = EDGE_CURVE ( 'NONE', #11758, #8061, #14117, .T. ) ;
#7758 = DIRECTION ( 'NONE',  ( -1.000000000000000000, -0.000000000000000000, -0.000000000000000000 ) ) ;
#7759 = FACE_OUTER_BOUND ( 'NONE', #10761, .T. ) ;
#7760 = CARTESIAN_POINT ( 'NONE',  ( -0.004184981454872216226, -0.1778800751599175500, 0.007038468095566932821 ) ) ;
#7761 = ADVANCED_FACE ( 'NONE', ( #9192 ), #4312, .F. ) ;
#7762 = CARTESIAN_POINT ( 'NONE',  ( 0.7455328141524921737, 1.190944881889763884, 0.3622425942646917418 ) ) ;
#7763 = DIRECTION ( 'NONE',  ( 0.000000000000000000, 1.000000000000000000, -0.000000000000000000 ) ) ;
#7764 = ORIENTED_EDGE ( 'NONE', *, *, #14092, .F. ) ;
#7765 = ADVANCED_FACE ( 'NONE', ( #13887 ), #14625, .T. ) ;
#7766 = VERTEX_POINT ( 'NONE', #4484 ) ;
#7767 = ORIENTED_EDGE ( 'NONE', *, *, #1543, .T. ) ;
#7768 = DIRECTION ( 'NONE',  ( -0.8660254037844385966, 0.000000000000000000, -0.5000000000000001110 ) ) ;
#7769 = CARTESIAN_POINT ( 'NONE',  ( -0.06867854503139178557, 0.1655849054964023959, -0.03830121270948787238 ) ) ;
#7770 = DIRECTION ( 'NONE',  ( -0.000000000000000000, -0.000000000000000000, -1.000000000000000000 ) ) ;
#7771 = LENGTH_MEASURE_WITH_UNIT ( LENGTH_MEASURE( 0.02539999999999999897 ), #13662 );
#7772 = CARTESIAN_POINT ( 'NONE',  ( -1.100415514366371861, -0.04998955061625905139, -0.03937007874015747977 ) ) ;
#7773 = FACE_OUTER_BOUND ( 'NONE', #8363, .T. ) ;
#7774 = VERTEX_POINT ( 'NONE', #7145 ) ;
#7775 = EDGE_CURVE ( 'NONE', #13421, #15234, #12816, .T. ) ;
#7776 = CARTESIAN_POINT ( 'NONE',  ( -1.332606523864378945, 0.1355266887446167634, 0.03937007874015747977 ) ) ;
#7777 = EDGE_CURVE ( 'NONE', #8855, #8643, #13123, .T. ) ;
#7778 = CARTESIAN_POINT ( 'NONE',  ( -0.2353927734918962178, -0.09842519685039370636, 0.06771310446496157931 ) ) ;
#7779 = ORIENTED_EDGE ( 'NONE', *, *, #14246, .F. ) ;
#7780 = ORIENTED_EDGE ( 'NONE', *, *, #11119, .T. ) ;
#7781 = EDGE_CURVE ( 'NONE', #14360, #5195, #7350, .T. ) ;
#7782 = CARTESIAN_POINT ( 'NONE',  ( 0.7052242655755273093, -1.858423098537180129, -0.08366141732283417787 ) ) ;
#7783 = EDGE_LOOP ( 'NONE', ( #6387, #8306 ) ) ;
#7784 = ORIENTED_EDGE ( 'NONE', *, *, #182, .T. ) ;
#7785 = SHAPE_REPRESENTATION ( 'Bolt', ( #11481 ), #14478 ) ;
#7786 = CARTESIAN_POINT ( 'NONE',  ( -1.398495881576244493, -0.02731002314121873387, 0.1968503937007874127 ) ) ;
#7787 = CARTESIAN_POINT ( 'NONE',  ( -1.988605610277403679, -2.761836062270417447, 0.1772901849371437688 ) ) ;
#7788 =( CONVERSION_BASED_UNIT ( 'INCH', #14942 ) LENGTH_UNIT ( ) NAMED_UNIT ( #7054 ) );
#7789 = CARTESIAN_POINT ( 'NONE',  ( 0.2325106836984822400, -0.1023622047244094474, 0.06483101467147835140 ) ) ;
#7790 = APPLICATION_CONTEXT ( 'automotive_design' ) ;
#7791 = CARTESIAN_POINT ( 'NONE',  ( -1.977730146514584009, -2.850383346250469518, -0.1596058012727677722 ) ) ;
#7792 = DIRECTION ( 'NONE',  ( 0.8660254037844405950, 0.000000000000000000, 0.4999999999999966693 ) ) ;
#7793 = CARTESIAN_POINT ( 'NONE',  ( 0.08199009355444122904, 0.06963377358818914620, 0.01990370102563883067 ) ) ;
#7794 = ADVANCED_FACE ( 'NONE', ( #9570 ), #7112, .T. ) ;
#7795 = FACE_BOUND ( 'NONE', #5179, .T. ) ;
#7796 = CARTESIAN_POINT ( 'NONE',  ( -2.084722658870310941, -1.679497184253527120, -0.1033551916919345920 ) ) ;
#7797 = ORIENTED_EDGE ( 'NONE', *, *, #4978, .F. ) ;
#7798 = EDGE_CURVE ( 'NONE', #13695, #9820, #122, .T. ) ;
#7799 = VERTEX_POINT ( 'NONE', #4947 ) ;
#7800 = ADVANCED_FACE ( 'NONE', ( #10809 ), #12075, .F. ) ;
#7801 = ORIENTED_EDGE ( 'NONE', *, *, #2616, .T. ) ;
#7802 = ORIENTED_EDGE ( 'NONE', *, *, #9695, .T. ) ;
#7803 = CARTESIAN_POINT ( 'NONE',  ( 1.928577636452524610E-17, -0.4921259842519685179, -0.1574803149606299191 ) ) ;
#7804 = EDGE_CURVE ( 'NONE', #9228, #13529, #27, .T. ) ;
#7805 = LINE ( 'NONE', #1718, #825 ) ;
#7806 = DIRECTION ( 'NONE',  ( 0.000000000000000000, 1.000000000000000000, 0.000000000000000000 ) ) ;
#7807 = CARTESIAN_POINT ( 'NONE',  ( -0.4552518684890389800, -0.1023622047244094474, 0.3855835468379172903 ) ) ;
#7808 = CARTESIAN_POINT ( 'NONE',  ( -2.184126211765463399, -1.902526540362047491, 0.08609155816397294492 ) ) ;
#7809 = DIRECTION ( 'NONE',  ( -0.000000000000000000, -1.000000000000000000, -0.000000000000000000 ) ) ;
#7810 = DIRECTION ( 'NONE',  ( -0.000000000000000000, 1.000000000000000000, 0.000000000000000000 ) ) ;
#7811 = CARTESIAN_POINT ( 'NONE',  ( -0.2681506793016945611, -0.4921259842519685179, 0.03207310886158504931 ) ) ;
#7812 = CYLINDRICAL_SURFACE ( 'NONE', #13944, 0.1574803149606299191 ) ;
#7813 = FACE_OUTER_BOUND ( 'NONE', #7866, .T. ) ;
#7814 = ORIENTED_EDGE ( 'NONE', *, *, #5438, .F. ) ;
#7815 = CARTESIAN_POINT ( 'NONE',  ( -2.073879752374872432, -2.575632606089756305, -0.1529717276817058880 ) ) ;
#7816 = CARTESIAN_POINT ( 'NONE',  ( 8.825956286652729502E-18, 0.07874015748031495954, 0.05298991407461853265 ) ) ;
#7817 = ORIENTED_EDGE ( 'NONE', *, *, #12751, .F. ) ;
#7818 = EDGE_LOOP ( 'NONE', ( #14976, #9696, #10013, #8385 ) ) ;
#7819 = PRODUCT_DEFINITION_CONTEXT ( 'detailed design', #7790, 'design' ) ;
#7820 = ORIENTED_EDGE ( 'NONE', *, *, #1743, .F. ) ;
#7821 = CIRCLE ( 'NONE', #6300, 0.01968503937007879193 ) ;
#7822 = TOROIDAL_SURFACE ( 'NONE', #6302, 0.03543307086614173179, 0.003937007874015747977 ) ;
#7823 = EDGE_CURVE ( 'NONE', #1544, #3165, #8400, .T. ) ;
#7824 = CIRCLE ( 'NONE', #8576, 0.1240157480314959260 ) ;
#7825 = CARTESIAN_POINT ( 'NONE',  ( 0.000000000000000000, 0.000000000000000000, 0.000000000000000000 ) ) ;
#7826 = DIRECTION ( 'NONE',  ( -0.000000000000000000, -1.000000000000000000, -0.000000000000000000 ) ) ;
#7827 = CYLINDRICAL_SURFACE ( 'NONE', #11207, 0.003937007874015737569 ) ;
#7828 = CARTESIAN_POINT ( 'NONE',  ( -1.182069932166307291, 0.3415656170906546940, -0.04962985469592846172 ) ) ;
#7829 = VERTEX_POINT ( 'NONE', #11781 ) ;
#7830 = CARTESIAN_POINT ( 'NONE',  ( 1.181102362204724310, -0.1240157480314955790, -0.02559055118110236185 ) ) ;
#7831 = DIRECTION ( 'NONE',  ( -0.000000000000000000, -1.000000000000000000, -0.000000000000000000 ) ) ;
#7832 = VECTOR ( 'NONE', #10084, 39.37007874015748143 ) ;
#7833 = VECTOR ( 'NONE', #279, 39.37007874015748143 ) ;
#7834 = CARTESIAN_POINT ( 'NONE',  ( -1.392039366404614897, -0.02281013714037220461, -0.03937007874015750752 ) ) ;
#7835 = FACE_OUTER_BOUND ( 'NONE', #2852, .T. ) ;
#7836 = EDGE_LOOP ( 'NONE', ( #2279, #6786 ) ) ;
#7837 = AXIS2_PLACEMENT_3D ( 'NONE', #5636, #5485, #4394 ) ;
#7838 = CYLINDRICAL_SURFACE ( 'NONE', #9438, 0.003937007874015758385 ) ;
#7839 = AXIS2_PLACEMENT_3D ( 'NONE', #2618, #12194, #13503 ) ;
#7840 = ORIENTED_EDGE ( 'NONE', *, *, #2182, .F. ) ;
#7841 = ORIENTED_EDGE ( 'NONE', *, *, #2365, .T. ) ;
#7842 = ORIENTED_EDGE ( 'NONE', *, *, #8447, .F. ) ;
#7843 = DIRECTION ( 'NONE',  ( 0.000000000000000000, 0.000000000000000000, 1.000000000000000000 ) ) ;
#7844 = PLANE ( 'NONE',  #10399 ) ;
#7845 = CIRCLE ( 'NONE', #1107, 0.03937007874015751446 ) ;
#7846 = TOROIDAL_SURFACE ( 'NONE', #1344, 0.2165354330708662012, 0.01968503937007873988 ) ;
#7847 = AXIS2_PLACEMENT_3D ( 'NONE', #7807, #5982, #9687 ) ;
#7848 = FACE_BOUND ( 'NONE', #8703, .T. ) ;
#7849 = CARTESIAN_POINT ( 'NONE',  ( 1.181102362204724310, 0.1240157480314959815, 0.02952755905511811330 ) ) ;
#7850 = AXIS2_PLACEMENT_3D ( 'NONE', #11509, #8844, #15038 ) ;
#7851 = DIRECTION ( 'NONE',  ( -0.8660254037844388186, 0.000000000000000000, 0.4999999999999995559 ) ) ;
#7852 = LINE ( 'NONE', #7940, #11626 ) ;
#7853 = ORIENTED_EDGE ( 'NONE', *, *, #145, .T. ) ;
#7854 = DIRECTION ( 'NONE',  ( 0.8660254037844389297, 0.000000000000000000, -0.4999999999999994449 ) ) ;
#7855 = ADVANCED_FACE ( 'NONE', ( #14440 ), #9078, .T. ) ;
#7856 = CARTESIAN_POINT ( 'NONE',  ( -0.1724006475077544398, -0.4921259842519685179, 0.1768186671464649640 ) ) ;
#7857 = DIRECTION ( 'NONE',  ( -0.000000000000000000, -0.000000000000000000, -1.000000000000000000 ) ) ;
#7858 = EDGE_LOOP ( 'NONE', ( #14501, #12249, #11743, #2871, #5218 ) ) ;
#7859 = AXIS2_PLACEMENT_3D ( 'NONE', #5460, #7973, #1949 ) ;
#7860 = AXIS2_PLACEMENT_3D ( 'NONE', #6105, #8249, #11849 ) ;
#7861 = ORIENTED_EDGE ( 'NONE', *, *, #9047, .F. ) ;
#7862 = VECTOR ( 'NONE', #10567, 39.37007874015748143 ) ;
#7863 = CIRCLE ( 'NONE', #1128, 0.03937007874015747977 ) ;
#7864 = ORIENTED_EDGE ( 'NONE', *, *, #409, .T. ) ;
#7865 = AXIS2_PLACEMENT_3D ( 'NONE', #568, #7706, #11537 ) ;
#7866 = EDGE_LOOP ( 'NONE', ( #3566, #12610, #13052, #4010 ) ) ;
#7867 = CIRCLE ( 'NONE', #4207, 0.5826771653543306728 ) ;
#7868 = EDGE_CURVE ( 'NONE', #12353, #6007, #6592, .T. ) ;
#7869 = DIRECTION ( 'NONE',  ( 1.000000000000000000, 8.673617379884029309E-17, -0.000000000000000000 ) ) ;
#7870 = CARTESIAN_POINT ( 'NONE',  ( -2.090051324975654268, -1.858423098536573503, -0.08664193191035729491 ) ) ;
#7871 = LENGTH_MEASURE_WITH_UNIT ( LENGTH_MEASURE( 0.02539999999999999897 ), #11310 );
#7872 = VECTOR ( 'NONE', #5111, 39.37007874015748143 ) ;
#7873 = VECTOR ( 'NONE', #10365, 39.37007874015748143 ) ;
#7874 = DIRECTION ( 'NONE',  ( -1.000000000000000000, 5.204170427930430118E-14, -0.000000000000000000 ) ) ;
#7875 = AXIS2_PLACEMENT_3D ( 'NONE', #10974, #1203, #5007 ) ;
#7876 = ADVANCED_FACE ( 'NONE', ( #2305 ), #3563, .T. ) ;
#7877 = CARTESIAN_POINT ( 'NONE',  ( -1.944102467919452959, -2.896447668998575420, -0.1270282496954552864 ) ) ;
#7878 = DIRECTION ( 'NONE',  ( 1.000000000000000000, 0.000000000000000000, 0.000000000000000000 ) ) ;
#7879 = CIRCLE ( 'NONE', #9131, 0.05905511811023620578 ) ;
#7880 = CARTESIAN_POINT ( 'NONE',  ( 0.000000000000000000, 1.622047244094488638, -0.5511811023622046335 ) ) ;
#7881 = CARTESIAN_POINT ( 'NONE',  ( -2.156935286759944503, -2.012462723082549587, -0.1097304796145708444 ) ) ;
#7882 = DIRECTION ( 'NONE',  ( 0.000000000000000000, -0.000000000000000000, 1.000000000000000000 ) ) ;
#7883 = VERTEX_POINT ( 'NONE', #5673 ) ;
#7884 = ORIENTED_EDGE ( 'NONE', *, *, #7603, .F. ) ;
#7885 = CIRCLE ( 'NONE', #892, 0.005905511811023620231 ) ;
#7886 = EDGE_LOOP ( 'NONE', ( #15137, #4767 ) ) ;
#7887 = CIRCLE ( 'NONE', #6131, 0.003937007874015724558 ) ;
#7888 = EDGE_LOOP ( 'NONE', ( #11959, #5231, #427, #4599 ) ) ;
#7889 = ADVANCED_FACE ( 'NONE', ( #1067 ), #4747, .T. ) ;
#7890 = VECTOR ( 'NONE', #6171, 39.37007874015748143 ) ;
#7891 = EDGE_CURVE ( 'NONE', #9354, #9753, #7082, .T. ) ;
#7892 = CARTESIAN_POINT ( 'NONE',  ( 0.07118569129171406495, 0.07239639532897740315, -0.03365426801084208525 ) ) ;
#7893 = PLANE ( 'NONE',  #6344 ) ;
#7894 = FACE_OUTER_BOUND ( 'NONE', #14523, .T. ) ;
#7895 = CARTESIAN_POINT ( 'NONE',  ( 0.4787092522273704853, 1.341768146560826658, 0.3474236500605594191 ) ) ;
#7896 = EDGE_CURVE ( 'NONE', #13132, #1093, #367, .T. ) ;
#7897 = CARTESIAN_POINT ( 'NONE',  ( -0.3137366569588388998, -0.2952755905511811330, 0.2947875711430708590 ) ) ;
#7898 = ADVANCED_FACE ( 'NONE', ( #6846 ), #4506, .T. ) ;
#7899 = AXIS2_PLACEMENT_3D ( 'NONE', #6224, #2780, #13371 ) ;
#7900 = LINE ( 'NONE', #6632, #8438 ) ;
#7901 = CARTESIAN_POINT ( 'NONE',  ( -1.931770777078986034, -2.785713767061171353, -0.1768904282990497179 ) ) ;
#7902 = AXIS2_PLACEMENT_3D ( 'NONE', #1815, #2830, #6437 ) ;
#7903 = EDGE_LOOP ( 'NONE', ( #7499, #5151, #3761, #11138 ) ) ;
#7904 = CARTESIAN_POINT ( 'NONE',  ( -1.398125690441303526, -0.003404927804347302606, 0.03937007874015747977 ) ) ;
#7905 = DIRECTION ( 'NONE',  ( 0.000000000000000000, 0.000000000000000000, -1.000000000000000000 ) ) ;
#7906 = CIRCLE ( 'NONE', #3409, 0.1279527559055117780 ) ;
#7907 = ORIENTED_EDGE ( 'NONE', *, *, #5790, .F. ) ;
#7908 = ORIENTED_EDGE ( 'NONE', *, *, #9935, .F. ) ;
#7909 = ORIENTED_EDGE ( 'NONE', *, *, #1352, .T. ) ;
#7910 = CIRCLE ( 'NONE', #678, 0.003937007874015758385 ) ;
#7911 = DIRECTION ( 'NONE',  ( 1.224646799147353207E-16, 1.000000000000000000, 0.000000000000000000 ) ) ;
#7912 = VECTOR ( 'NONE', #3871, 39.37007874015748143 ) ;
#7913 = CYLINDRICAL_SURFACE ( 'NONE', #3860, 0.003937007874015724558 ) ;
#7914 = DIRECTION ( 'NONE',  ( -1.060575238724906668E-16, 1.000000000000000000, -6.123233995736768501E-17 ) ) ;
#7915 = EDGE_CURVE ( 'NONE', #13903, #14791, #10621, .T. ) ;
#7916 = CARTESIAN_POINT ( 'NONE',  ( -0.1062992125983148878, -0.1023622047244094474, -0.5909884645248143498 ) ) ;
#7917 = DIRECTION ( 'NONE',  ( -0.000000000000000000, 1.000000000000000000, 0.000000000000000000 ) ) ;
#7918 = VERTEX_POINT ( 'NONE', #10387 ) ;
#7919 = LINE ( 'NONE', #9092, #11949 ) ;
#7920 = CARTESIAN_POINT ( 'NONE',  ( 0.5413385826771386355, -0.09448818897637796532, 0.2443509997554994817 ) ) ;
#7921 = AXIS2_PLACEMENT_3D ( 'NONE', #10691, #8321, #4417 ) ;
#7922 = DIRECTION ( 'NONE',  ( 0.000000000000000000, 0.000000000000000000, -1.000000000000000000 ) ) ;
#7923 = EDGE_CURVE ( 'NONE', #8061, #1797, #10542, .T. ) ;
#7924 = FACE_OUTER_BOUND ( 'NONE', #15328, .T. ) ;
#7925 = EDGE_LOOP ( 'NONE', ( #4048, #12270, #4662, #3415 ) ) ;
#7926 = EDGE_CURVE ( 'NONE', #9877, #10603, #1123, .T. ) ;
#7927 = DIRECTION ( 'NONE',  ( 0.000000000000000000, 0.000000000000000000, 1.000000000000000000 ) ) ;
#7928 = AXIS2_PLACEMENT_3D ( 'NONE', #3631, #2368, #7151 ) ;
#7929 = VERTEX_POINT ( 'NONE', #9533 ) ;
#7930 = VERTEX_POINT ( 'NONE', #3329 ) ;
#7931 = ORIENTED_EDGE ( 'NONE', *, *, #8024, .T. ) ;
#7932 = VECTOR ( 'NONE', #10883, 39.37007874015748143 ) ;
#7933 = DIRECTION ( 'NONE',  ( 0.000000000000000000, 0.000000000000000000, 1.000000000000000000 ) ) ;
#7934 = CARTESIAN_POINT ( 'NONE',  ( 0.5871416322685650835, 0.000000000000000000, 0.1571437749735215272 ) ) ;
#7935 = CARTESIAN_POINT ( 'NONE',  ( -0.04751022371103294506, 0.1688405673728649303, -0.05319490010182324757 ) ) ;
#7936 = CARTESIAN_POINT ( 'NONE',  ( 0.000000000000000000, 1.417322834645669438, -0.6614173228346456046 ) ) ;
#7937 = ITEM_DEFINED_TRANSFORMATION ( 'NONE', 'NONE', #5347,  #11481 ) ;
#7938 = DIRECTION ( 'NONE',  ( 0.000000000000000000, -1.000000000000000000, 0.000000000000000000 ) ) ;
#7939 = AXIS2_PLACEMENT_3D ( 'NONE', #4827, #14485, #2415 ) ;
#7940 = CARTESIAN_POINT ( 'NONE',  ( -0.5905511811023629321, -0.09448818897637796532, 0.1591122789105256785 ) ) ;
#7941 = ORIENTED_EDGE ( 'NONE', *, *, #13481, .T. ) ;
#7942 = DIRECTION ( 'NONE',  ( 1.000000000000000000, 0.000000000000000000, -0.000000000000000000 ) ) ;
#7943 = FACE_OUTER_BOUND ( 'NONE', #9225, .T. ) ;
#7944 = CIRCLE ( 'NONE', #7196, 0.01968503937007874335 ) ;
#7945 = CARTESIAN_POINT ( 'NONE',  ( -1.181342415325335571, 0.3435647566446752288, -0.04457062106905999854 ) ) ;
#7946 = FACE_OUTER_BOUND ( 'NONE', #13755, .T. ) ;
#7947 = CIRCLE ( 'NONE', #12964, 0.007874015748031449116 ) ;
#7948 = ORIENTED_EDGE ( 'NONE', *, *, #9830, .F. ) ;
#7949 = CARTESIAN_POINT ( 'NONE',  ( -0.6582248459352179060, -0.2952755905511811330, -0.3018834747714004840 ) ) ;
#7950 = ORIENTED_EDGE ( 'NONE', *, *, #6473, .T. ) ;
#7951 = AXIS2_PLACEMENT_3D ( 'NONE', #8286, #5136, #9849 ) ;
#7952 = ORIENTED_EDGE ( 'NONE', *, *, #9530, .F. ) ;
#7953 = DIRECTION ( 'NONE',  ( -0.000000000000000000, -0.000000000000000000, -1.000000000000000000 ) ) ;
#7954 = CARTESIAN_POINT ( 'NONE',  ( 0.000000000000000000, 0.5905511811023621549, -0.5984251968503937480 ) ) ;
#7955 = CIRCLE ( 'NONE', #4459, 0.003937007874015724558 ) ;
#7956 = SPHERICAL_SURFACE ( 'NONE', #2705, 0.003937007874015747977 ) ;
#7957 = LINE ( 'NONE', #6609, #13577 ) ;
#7958 = AXIS2_PLACEMENT_3D ( 'NONE', #2897, #1729, #5297 ) ;
#7959 = CARTESIAN_POINT ( 'NONE',  ( 0.05905511811023622659, 1.190944881889763884, -0.8267716535433072833 ) ) ;
#7960 = EDGE_CURVE ( 'NONE', #3213, #9228, #15249, .T. ) ;
#7961 = CARTESIAN_POINT ( 'NONE',  ( -1.568343923620152180, 0.1178486908565801600, 0.03937007874015747977 ) ) ;
#7962 = DIRECTION ( 'NONE',  ( 0.000000000000000000, 0.000000000000000000, 1.000000000000000000 ) ) ;
#7963 = ADVANCED_FACE ( 'NONE', ( #5817 ), #12980, .T. ) ;
#7964 = ORIENTED_EDGE ( 'NONE', *, *, #4380, .F. ) ;
#7965 = EDGE_LOOP ( 'NONE', ( #5075, #14684, #5480, #11833, #1676, #5122, #13966 ) ) ;
#7966 = VECTOR ( 'NONE', #11573, 39.37007874015748143 ) ;
#7967 = ORIENTED_EDGE ( 'NONE', *, *, #9597, .T. ) ;
#7968 = ORIENTED_EDGE ( 'NONE', *, *, #4819, .T. ) ;
#7969 = ADVANCED_FACE ( 'NONE', ( #11803 ), #15410, .T. ) ;
#7970 = DIRECTION ( 'NONE',  ( -1.000000000000000000, -0.000000000000000000, -3.614007241618347785E-16 ) ) ;
#7971 = CARTESIAN_POINT ( 'NONE',  ( -0.06692913385815749128, -0.1023622047244094474, -0.2377126739438355507 ) ) ;
#7972 = CARTESIAN_POINT ( 'NONE',  ( 0.5905511811023622659, -0.2952755905511811330, -0.4190977005962939206 ) ) ;
#7973 = DIRECTION ( 'NONE',  ( 1.000000000000000000, 0.000000000000000000, -1.224646799147353207E-16 ) ) ;
#7974 = CARTESIAN_POINT ( 'NONE',  ( 0.000000000000000000, 0.5511811023622046335, 0.6614173228346456046 ) ) ;
#7975 = FACE_OUTER_BOUND ( 'NONE', #3488, .T. ) ;
#7976 = DIRECTION ( 'NONE',  ( 0.8660254037844383745, 0.000000000000000000, 0.5000000000000004441 ) ) ;
#7977 = VERTEX_POINT ( 'NONE', #8271 ) ;
#7978 = CARTESIAN_POINT ( 'NONE',  ( 0.1724006475077543565, -0.4921259842519685179, 0.1728816592724491952 ) ) ;
#7979 = ADVANCED_FACE ( 'NONE', ( #1157 ), #1615, .T. ) ;
#7980 = DIRECTION ( 'NONE',  ( 0.8660254037844395958, 0.000000000000000000, 0.4999999999999982236 ) ) ;
#7981 = CARTESIAN_POINT ( 'NONE',  ( 4.339299682018179909E-18, 0.4094488188976377896, -0.03543307086614173179 ) ) ;
#7982 = EDGE_CURVE ( 'NONE', #14238, #14162, #7609, .T. ) ;
#7983 = ORIENTED_EDGE ( 'NONE', *, *, #3722, .T. ) ;
#7984 =( BOUNDED_SURFACE ( )  B_SPLINE_SURFACE ( 3, 2, ( 
 ( #4175, #6270, #5251 ),
 ( #7468, #3950, #12410 ),
 ( #2930, #8970, #432 ),
 ( #12491, #345, #14922 ),
 ( #9824, #8795, #11382 ),
 ( #8884, #567, #7533 ),
 ( #6438, #14691, #13563 ),
 ( #14601, #6352, #13427 ),
 ( #13497, #1681, #11230 ),
 ( #3866, #12260, #13661 ) ),
 .UNSPECIFIED., .F., .F., .T. ) 
 B_SPLINE_SURFACE_WITH_KNOTS ( ( 4, 2, 2, 2, 4 ),
 ( 3, 3 ),
 ( 0.000000000000000000, 0.01438918893332945780, 0.02158378339999418583, 0.02518108063332655244, 0.02877837786665891559 ),
 ( 0.000000000000000000, 1.000000000000000000 ),
 .UNSPECIFIED. ) 
 GEOMETRIC_REPRESENTATION_ITEM ( )  RATIONAL_B_SPLINE_SURFACE ( (
 ( 1.000000000000000000, 0.7071067811865475727, 1.000000000000000000),
 ( 1.000000000000000000, 0.7064777154098520473, 1.000000000000000000),
 ( 1.000000000000000000, 0.7074394717099544705, 1.000000000000000000),
 ( 1.000000000000000000, 0.7110974249889780996, 1.000000000000000000),
 ( 1.000000000000000000, 0.7126855531371033559, 1.000000000000000000),
 ( 1.000000000000000000, 0.7155933398974227977, 1.000000000000000000),
 ( 1.000000000000000000, 0.7166513996729255709, 1.000000000000000000),
 ( 1.000000000000000000, 0.7189195979667037939, 1.000000000000000000),
 ( 1.000000000000000000, 0.7201312545562511547, 1.000000000000000000),
 ( 1.000000000000000000, 0.7214151048184016535, 1.000000000000000000) ) ) 
 REPRESENTATION_ITEM ( '' )  SURFACE ( )  );
#7985 = ORIENTED_EDGE ( 'NONE', *, *, #5571, .T. ) ;
#7986 = EDGE_CURVE ( 'NONE', #11452, #8847, #216, .T. ) ;
#7987 = ADVANCED_FACE ( 'NONE', ( #6136, #3732, #3797 ), #1298, .F. ) ;
#7988 = ORIENTED_EDGE ( 'NONE', *, *, #1858, .T. ) ;
#7989 = LINE ( 'NONE', #12769, #15122 ) ;
#7990 = CARTESIAN_POINT ( 'NONE',  ( -1.181342415325333350, 0.3435647566446739520, 0.03937007874015747977 ) ) ;
#7991 = LINE ( 'NONE', #10657, #14894 ) ;
#7992 = DIRECTION ( 'NONE',  ( 0.000000000000000000, 0.000000000000000000, 1.000000000000000000 ) ) ;
#7993 = DIRECTION ( 'NONE',  ( 0.8660254037844385966, -0.000000000000000000, 0.5000000000000001110 ) ) ;
#7994 = VERTEX_POINT ( 'NONE', #7174 ) ;
#7995 = LINE ( 'NONE', #5633, #14939 ) ;
#7996 = FACE_OUTER_BOUND ( 'NONE', #4489, .T. ) ;
#7997 = CARTESIAN_POINT ( 'NONE',  ( -0.05905511811023622659, 1.338582677165354395, -0.5955041639236611228 ) ) ;
#7998 = FACE_OUTER_BOUND ( 'NONE', #9198, .T. ) ;
#7999 = ORIENTED_EDGE ( 'NONE', *, *, #10185, .T. ) ;
#8000 = DIRECTION ( 'NONE',  ( -0.000000000000000000, -2.212657494868377674E-16, 1.000000000000000000 ) ) ;
#8001 = EDGE_LOOP ( 'NONE', ( #8572, #13050, #7255, #12523 ) ) ;
#8002 = ADVANCED_FACE ( 'NONE', ( #9691 ), #2116, .T. ) ;
#8003 = ADVANCED_FACE ( 'NONE', ( #2704 ), #3858, .T. ) ;
#8004 = EDGE_LOOP ( 'NONE', ( #10606, #12815 ) ) ;
#8005 = EDGE_LOOP ( 'NONE', ( #11744, #9421, #1738, #5637 ) ) ;
#8006 = FACE_OUTER_BOUND ( 'NONE', #7369, .T. ) ;
#8007 = DIRECTION ( 'NONE',  ( 0.000000000000000000, -0.000000000000000000, -1.000000000000000000 ) ) ;
#8008 = EDGE_CURVE ( 'NONE', #4713, #2230, #11359, .T. ) ;
#8009 = DIRECTION ( 'NONE',  ( -0.000000000000000000, -0.000000000000000000, -1.000000000000000000 ) ) ;
#8010 = DIRECTION ( 'NONE',  ( 4.336808689942006376E-14, 0.000000000000000000, -1.000000000000000000 ) ) ;
#8011 = SHAPE_DEFINITION_REPRESENTATION ( #15291, #6262 ) ;
#8012 = DIRECTION ( 'NONE',  ( 0.8660254037844388186, -0.000000000000000000, -0.4999999999999995559 ) ) ;
#8013 = DIRECTION ( 'NONE',  ( -1.000000000000000000, -0.000000000000000000, -3.614007241618347785E-16 ) ) ;
#8014 = ORIENTED_EDGE ( 'NONE', *, *, #7160, .T. ) ;
#8015 = DIRECTION ( 'NONE',  ( 0.000000000000000000, 0.000000000000000000, 1.000000000000000000 ) ) ;
#8016 = LINE ( 'NONE', #8257, #12385 ) ;
#8017 = CARTESIAN_POINT ( 'NONE',  ( -0.05314960629918528967, -0.09842519685039370636, -0.09205781851247189784 ) ) ;
#8018 = ORIENTED_EDGE ( 'NONE', *, *, #8292, .T. ) ;
#8019 = VERTEX_POINT ( 'NONE', #4969 ) ;
#8020 = CARTESIAN_POINT ( 'NONE',  ( -0.4751993499419962519, 1.035433070866141891, 0.3506226965216301950 ) ) ;
#8021 = VERTEX_POINT ( 'NONE', #13277 ) ;
#8022 = VERTEX_POINT ( 'NONE', #7475 ) ;
#8023 = ORIENTED_EDGE ( 'NONE', *, *, #4857, .F. ) ;
#8024 = EDGE_CURVE ( 'NONE', #11911, #12552, #133, .T. ) ;
#8025 = CARTESIAN_POINT ( 'NONE',  ( -0.5595825771504281398, -0.09842519685039372024, 0.2048774586467239645 ) ) ;
#8026 = CARTESIAN_POINT ( 'NONE',  ( -1.962370792254545027, -2.889990620475674898, 0.1128190176297459296 ) ) ;
#8027 = PRODUCT ( 'Finger', 'Finger', '', ( #4250 ) ) ;
#8028 = FACE_OUTER_BOUND ( 'NONE', #10822, .T. ) ;
#8029 = DIRECTION ( 'NONE',  ( -0.000000000000000000, -1.000000000000000000, -0.000000000000000000 ) ) ;
#8030 = CARTESIAN_POINT ( 'NONE',  ( -1.398125690441303526, -0.003404927804347094439, 0.05905511811023622659 ) ) ;
#8031 = LINE ( 'NONE', #9465, #5303 ) ;
#8032 = DIRECTION ( 'NONE',  ( -0.000000000000000000, -1.000000000000000000, -0.000000000000000000 ) ) ;
#8033 = ORIENTED_EDGE ( 'NONE', *, *, #352, .T. ) ;
#8034 = ORIENTED_EDGE ( 'NONE', *, *, #3179, .T. ) ;
#8035 = ORIENTED_EDGE ( 'NONE', *, *, #5609, .T. ) ;
#8036 = VERTEX_POINT ( 'NONE', #11970 ) ;
#8037 = DIRECTION ( 'NONE',  ( 1.000000000000000000, 0.000000000000000000, 0.000000000000000000 ) ) ;
#8038 = CARTESIAN_POINT ( 'NONE',  ( 0.06692913385832209572, -0.2952755905511811330, -0.4624047872104674606 ) ) ;
#8039 = EDGE_CURVE ( 'NONE', #8264, #2150, #5846, .T. ) ;
#8040 = CARTESIAN_POINT ( 'NONE',  ( 0.09061599198715353243, 0.06736074103232449206, 0.007444810018878659542 ) ) ;
#8041 = FACE_OUTER_BOUND ( 'NONE', #771, .T. ) ;
#8042 = FACE_OUTER_BOUND ( 'NONE', #13412, .T. ) ;
#8043 = CARTESIAN_POINT ( 'NONE',  ( 0.000000000000000000, 1.346456692913385877, 0.000000000000000000 ) ) ;
#8044 = CARTESIAN_POINT ( 'NONE',  ( -1.951077307720631149, -2.792367362670038045, -0.1761343083128099618 ) ) ;
#8045 = ORIENTED_EDGE ( 'NONE', *, *, #2458, .T. ) ;
#8046 = DIRECTION ( 'NONE',  ( 0.8660254037844383745, 0.000000000000000000, 0.5000000000000004441 ) ) ;
#8047 = EDGE_CURVE ( 'NONE', #13962, #13771, #12881, .T. ) ;
#8048 = CARTESIAN_POINT ( 'NONE',  ( -1.332606523864378945, 0.1355266887446167634, 0.05905511811023622659 ) ) ;
#8049 = DIRECTION ( 'NONE',  ( -0.9966420383350262924, 0.000000000000000000, -0.08188191145426275408 ) ) ;
#8050 = ORIENTED_EDGE ( 'NONE', *, *, #6229, .T. ) ;
#8051 = EDGE_LOOP ( 'NONE', ( #11625, #12424, #11650, #12888 ) ) ;
#8052 = ORIENTED_EDGE ( 'NONE', *, *, #6268, .T. ) ;
#8053 = LINE ( 'NONE', #10421, #3876 ) ;
#8054 = EDGE_CURVE ( 'NONE', #12616, #5709, #11628, .T. ) ;
#8055 = ADVANCED_FACE ( 'NONE', ( #5985 ), #2537, .F. ) ;
#8056 = DIRECTION ( 'NONE',  ( 0.000000000000000000, 0.000000000000000000, 1.000000000000000000 ) ) ;
#8057 = CARTESIAN_POINT ( 'NONE',  ( -1.925122157694118652, -2.949207805218784006, 0.01171943552855665704 ) ) ;
#8058 = FACE_OUTER_BOUND ( 'NONE', #1799, .T. ) ;
#8059 = DIRECTION ( 'NONE',  ( 1.000000000000000000, 8.673617379884013384E-15, 0.000000000000000000 ) ) ;
#8060 = LINE ( 'NONE', #11686, #3647 ) ;
#8061 = VERTEX_POINT ( 'NONE', #8659 ) ;
#8062 = CARTESIAN_POINT ( 'NONE',  ( 0.5403775172679829986, 1.038795175326499676, 0.2394877259645026013 ) ) ;
#8063 = EDGE_CURVE ( 'NONE', #9261, #6775, #13625, .T. ) ;
#8064 = CARTESIAN_POINT ( 'NONE',  ( 0.000000000000000000, 2.637795275590551825, 0.03937007874015747977 ) ) ;
#8065 = CARTESIAN_POINT ( 'NONE',  ( -0.02374036903667606571, 0.1505616924844531690, 0.03732860159234808323 ) ) ;
#8066 = DIRECTION ( 'NONE',  ( -0.000000000000000000, -1.000000000000000000, -0.000000000000000000 ) ) ;
#8067 = VERTEX_POINT ( 'NONE', #12106 ) ;
#8068 = DIRECTION ( 'NONE',  ( 1.000000000000000000, 0.000000000000000000, 0.000000000000000000 ) ) ;
#8069 = AXIS2_PLACEMENT_3D ( 'NONE', #14546, #12277, #1536 ) ;
#8070 = ORIENTED_EDGE ( 'NONE', *, *, #3717, .T. ) ;
#8071 = VERTEX_POINT ( 'NONE', #5033 ) ;
#8072 = ORIENTED_EDGE ( 'NONE', *, *, #6123, .F. ) ;
#8073 = ORIENTED_EDGE ( 'NONE', *, *, #317, .T. ) ;
#8074 = ADVANCED_FACE ( 'NONE', ( #9831 ), #10772, .F. ) ;
#8075 = FACE_OUTER_BOUND ( 'NONE', #7022, .T. ) ;
#8076 = CARTESIAN_POINT ( 'NONE',  ( -1.964126537190518107, -2.749515453455440905, 0.1756903148397124803 ) ) ;
#8077 = EDGE_CURVE ( 'NONE', #7421, #11540, #8126, .T. ) ;
#8078 = DIRECTION ( 'NONE',  ( -0.000000000000000000, -1.000000000000000000, -0.000000000000000000 ) ) ;
#8079 = CARTESIAN_POINT ( 'NONE',  ( 0.000000000000000000, 0.000000000000000000, 0.000000000000000000 ) ) ;
#8080 = CONTEXT_DEPENDENT_SHAPE_REPRESENTATION ( #13715, #13043 ) ;
#8081 = DIRECTION ( 'NONE',  ( 0.000000000000000000, 0.000000000000000000, 1.000000000000000000 ) ) ;
#8082 = VECTOR ( 'NONE', #14346, 39.37007874015748854 ) ;
#8083 = CIRCLE ( 'NONE', #12596, 0.6614173228346456046 ) ;
#8084 = DIRECTION ( 'NONE',  ( -0.000000000000000000, 1.000000000000000000, 0.000000000000000000 ) ) ;
#8085 = ORIENTED_EDGE ( 'NONE', *, *, #8852, .F. ) ;
#8086 = DIRECTION ( 'NONE',  ( 1.224646799147358384E-16, 0.000000000000000000, -1.000000000000000000 ) ) ;
#8087 = AXIS2_PLACEMENT_3D ( 'NONE', #2476, #2539, #1379 ) ;
#8088 = ADVANCED_FACE ( 'NONE', ( #14771 ), #10140, .T. ) ;
#8089 = AXIS2_PLACEMENT_3D ( 'NONE', #312, #7273, #2737 ) ;
#8090 = CARTESIAN_POINT ( 'NONE',  ( 0.06011003619072806392, -0.1023622047244094474, -0.2337756660697248301 ) ) ;
#8091 = DIRECTION ( 'NONE',  ( -0.8660254037844389297, -0.000000000000000000, 0.4999999999999994449 ) ) ;
#8092 = DIRECTION ( 'NONE',  ( 0.000000000000000000, 1.000000000000000000, 0.000000000000000000 ) ) ;
#8093 = ORIENTED_EDGE ( 'NONE', *, *, #5438, .T. ) ;
#8094 = EDGE_LOOP ( 'NONE', ( #5827, #13838, #13280, #3250 ) ) ;
#8095 = APPLICATION_CONTEXT ( 'automotive_design' ) ;
#8096 = EDGE_CURVE ( 'NONE', #9504, #3033, #13136, .T. ) ;
#8097 = CYLINDRICAL_SURFACE ( 'NONE', #4852, 0.003937007874015758385 ) ;
#8099 = ORIENTED_EDGE ( 'NONE', *, *, #11037, .T. ) ;
#8098 = AXIS2_PLACEMENT_3D ( 'NONE', #4195, #364, #2854 ) ;
#8100 = AXIS2_PLACEMENT_3D ( 'NONE', #2000, #4666, #11552 ) ;
#8101 = VERTEX_POINT ( 'NONE', #6680 ) ;
#8102 = AXIS2_PLACEMENT_3D ( 'NONE', #1199, #3464, #14193 ) ;
#8103 = ORIENTED_EDGE ( 'NONE', *, *, #2047, .F. ) ;
#8104 = AXIS2_PLACEMENT_3D ( 'NONE', #3228, #5634, #14987 ) ;
#8105 = CARTESIAN_POINT ( 'NONE',  ( -1.181102362204724310, 0.000000000000000000, 0.02559055118110236185 ) ) ;
#8106 = FACE_BOUND ( 'NONE', #11564, .T. ) ;
#8107 = CARTESIAN_POINT ( 'NONE',  ( -1.950291921842994158, -2.794930396112696336, -0.1760874378794451134 ) ) ;
#8108 = PLANE ( 'NONE',  #14218 ) ;
#8109 = DIRECTION ( 'NONE',  ( 1.000000000000000000, 0.000000000000000000, -1.224646799147353207E-16 ) ) ;
#8110 = CARTESIAN_POINT ( 'NONE',  ( 0.06299212598430639631, -0.4921259842519685179, -0.5870514566507987197 ) ) ;
#8111 = ADVANCED_FACE ( 'NONE', ( #2940, #1759 ), #5502, .T. ) ;
#8112 = CARTESIAN_POINT ( 'NONE',  ( -1.409467368996963010, -0.007141430561139886987, 0.06138464873084744505 ) ) ;
#8113 = AXIS2_PLACEMENT_3D ( 'NONE', #9266, #14044, #7224 ) ;
#8114 = AXIS2_PLACEMENT_3D ( 'NONE', #12413, #2534, #349 ) ;
#8115 = FACE_OUTER_BOUND ( 'NONE', #1006, .T. ) ;
#8116 = SURFACE_STYLE_FILL_AREA ( #4204 ) ;
#8117 = CIRCLE ( 'NONE', #360, 0.2303149606299203511 ) ;
#8118 = AXIS2_PLACEMENT_3D ( 'NONE', #2219, #11782, #14122 ) ;
#8119 = EDGE_CURVE ( 'NONE', #556, #8212, #7711, .T. ) ;
#8120 = VERTEX_POINT ( 'NONE', #6513 ) ;
#8121 = AXIS2_PLACEMENT_3D ( 'NONE', #9825, #3646, #14373 ) ;
#8122 = EDGE_CURVE ( 'NONE', #4524, #315, #512, .T. ) ;
#8123 = ORIENTED_EDGE ( 'NONE', *, *, #3126, .T. ) ;
#8124 = ORIENTED_EDGE ( 'NONE', *, *, #8047, .T. ) ;
#8125 = ORIENTED_EDGE ( 'NONE', *, *, #5843, .F. ) ;
#8126 = CIRCLE ( 'NONE', #14869, 0.03937007874015747977 ) ;
#8127 = CIRCLE ( 'NONE', #6104, 0.003937007874015724558 ) ;
#8128 = CARTESIAN_POINT ( 'NONE',  ( 4.821444091131316146E-18, 0.003937007874015749712, 0.03937007874015751446 ) ) ;
#8129 = DIRECTION ( 'NONE',  ( 0.5984233124757303290, 0.8011800915434521553, -0.000000000000000000 ) ) ;
#8130 = AXIS2_PLACEMENT_3D ( 'NONE', #12016, #10810, #99 ) ;
#8131 = FACE_OUTER_BOUND ( 'NONE', #13068, .T. ) ;
#8132 = CARTESIAN_POINT ( 'NONE',  ( -0.4854723491485721798, 1.043263280880422528, 0.3484785681409913738 ) ) ;
#8133 = CARTESIAN_POINT ( 'NONE',  ( -0.1618514667033796040, -0.4921259842519685179, 0.2083147301385909200 ) ) ;
#8134 = CARTESIAN_POINT ( 'NONE',  ( -0.5452755905511542656, -0.09842519685039370636, 0.2375319020879049503 ) ) ;
#8135 = DIRECTION ( 'NONE',  ( 0.000000000000000000, 0.000000000000000000, 1.000000000000000000 ) ) ;
#8136 = EDGE_LOOP ( 'NONE', ( #14842, #14955, #377, #4834 ) ) ;
#8137 = LINE ( 'NONE', #1017, #2684 ) ;
#8138 = CARTESIAN_POINT ( 'NONE',  ( 0.4803149606299220720, -0.4881889763779528324, 0.3500470136031578750 ) ) ;
#8139 = AXIS2_PLACEMENT_3D ( 'NONE', #14351, #8403, #13188 ) ;
#8140 = AXIS2_PLACEMENT_3D ( 'NONE', #13415, #6032, #14357 ) ;
#8141 = AXIS2_PLACEMENT_3D ( 'NONE', #3494, #8327, #14144 ) ;
#8142 = ORIENTED_EDGE ( 'NONE', *, *, #3219, .T. ) ;
#8143 = ORIENTED_EDGE ( 'NONE', *, *, #7518, .F. ) ;
#8144 = AXIS2_PLACEMENT_3D ( 'NONE', #7342, #8462, #2498 ) ;
#8145 = VERTEX_POINT ( 'NONE', #4182 ) ;
#8146 = DIRECTION ( 'NONE',  ( -0.4274092037376936992, 0.000000000000000000, -0.9040582794047685722 ) ) ;
#8147 = TOROIDAL_SURFACE ( 'NONE', #10895, 3.149606299212599048, 0.01968503937007873988 ) ;
#8148 = AXIS2_PLACEMENT_3D ( 'NONE', #6963, #15268, #9396 ) ;
#8149 = AXIS2_PLACEMENT_3D ( 'NONE', #6577, #5880, #971 ) ;
#8150 = DIRECTION ( 'NONE',  ( 0.000000000000000000, 1.734723475976817507E-14, -1.000000000000000000 ) ) ;
#8151 = LINE ( 'NONE', #2268, #8628 ) ;
#8152 = DIRECTION ( 'NONE',  ( -0.9387676358159492418, 0.3445509047216873677, 0.000000000000000000 ) ) ;
#8153 = FACE_OUTER_BOUND ( 'NONE', #2156, .T. ) ;
#8154 = VECTOR ( 'NONE', #9531, 39.37007874015748854 ) ;
#8155 = CARTESIAN_POINT ( 'NONE',  ( -0.4307978335858689278, -0.09842519685039370636, 0.4318761856142863120 ) ) ;
#8156 = ORIENTED_EDGE ( 'NONE', *, *, #3969, .T. ) ;
#8157 = DIRECTION ( 'NONE',  ( 0.5000000000000004441, 0.000000000000000000, -0.8660254037844383745 ) ) ;
#8158 = CARTESIAN_POINT ( 'NONE',  ( 0.5629921259843070347, -0.1023622047244094474, 0.2068459625837795746 ) ) ;
#8159 = DIRECTION ( 'NONE',  ( 0.5000000000000003331, 0.000000000000000000, -0.8660254037844385966 ) ) ;
#8160 = FACE_OUTER_BOUND ( 'NONE', #3110, .T. ) ;
#8161 = ORIENTED_EDGE ( 'NONE', *, *, #11637, .T. ) ;
#8162 = EDGE_CURVE ( 'NONE', #12485, #6809, #13883, .T. ) ;
#8163 = DIRECTION ( 'NONE',  ( 1.000000000000000000, 0.000000000000000000, 0.000000000000000000 ) ) ;
#8164 = AXIS2_PLACEMENT_3D ( 'NONE', #11379, #5719, #12555 ) ;
#8165 = CIRCLE ( 'NONE', #15417, 0.03937007874015751446 ) ;
#8166 = EDGE_CURVE ( 'NONE', #13305, #13509, #6445, .T. ) ;
#8167 = ORIENTED_EDGE ( 'NONE', *, *, #2906, .T. ) ;
#8168 = EDGE_LOOP ( 'NONE', ( #3338, #14906, #11865, #1765 ) ) ;
#8169 = ORIENTED_EDGE ( 'NONE', *, *, #1508, .T. ) ;
#8170 = CIRCLE ( 'NONE', #2404, 2.214566929133857887 ) ;
#8171 = PRODUCT ( 'Connecting Link', 'Connecting Link', '', ( #4177 ) ) ;
#8172 = ADVANCED_FACE ( 'NONE', ( #4025 ), #8801, .T. ) ;
#8173 = CARTESIAN_POINT ( 'NONE',  ( 0.4591888763630541104, -0.4881889763779528324, 0.3787644491703229810 ) ) ;
#8174 = DIRECTION ( 'NONE',  ( 0.8660254037844389297, 0.000000000000000000, -0.4999999999999996669 ) ) ;
#8175 = CARTESIAN_POINT ( 'NONE',  ( -0.002557446713253753914, 0.1765481709910071695, -0.0002437469044493141156 ) ) ;
#8176 = CARTESIAN_POINT ( 'NONE',  ( 0.1213717603336464113, 2.440944881889763884, -0.04263160285333145172 ) ) ;
#8177 = CONTEXT_DEPENDENT_SHAPE_REPRESENTATION ( #10502, #14039 ) ;
#8178 = DIRECTION ( 'NONE',  ( -1.000000000000000000, 0.000000000000000000, 0.000000000000000000 ) ) ;
#8179 = VECTOR ( 'NONE', #15233, 39.37007874015748143 ) ;
#8180 = CARTESIAN_POINT ( 'NONE',  ( -1.568343923620152847, 0.1178486908565804514, 0.05905511811023622659 ) ) ;
#8181 = ORIENTED_EDGE ( 'NONE', *, *, #7775, .F. ) ;
#8182 = CARTESIAN_POINT ( 'NONE',  ( -1.234181327013985197, 0.1355266887446167634, 0.05905511811023622659 ) ) ;
#8183 = CARTESIAN_POINT ( 'NONE',  ( 0.000000000000000000, 1.606299212598425674, 0.6614173228346456046 ) ) ;
#8184 = AXIS2_PLACEMENT_3D ( 'NONE', #1105, #10269, #6895 ) ;
#8185 = DIRECTION ( 'NONE',  ( 0.000000000000000000, 0.000000000000000000, 1.000000000000000000 ) ) ;
#8186 = DIRECTION ( 'NONE',  ( 0.5000000000000004441, 0.000000000000000000, 0.8660254037844383745 ) ) ;
#8187 = AXIS2_PLACEMENT_3D ( 'NONE', #6818, #7938, #11296 ) ;
#8188 = ORIENTED_EDGE ( 'NONE', *, *, #778, .F. ) ;
#8189 = EDGE_CURVE ( 'NONE', #6904, #4794, #4622, .T. ) ;
#8190 = ORIENTED_EDGE ( 'NONE', *, *, #6451, .F. ) ;
#8191 = CARTESIAN_POINT ( 'NONE',  ( 8.196454954923229282E-17, 0.5433070866141731514, 0.6692913385826770867 ) ) ;
#8192 = ORIENTED_EDGE ( 'NONE', *, *, #5290, .T. ) ;
#8193 = AXIS2_PLACEMENT_3D ( 'NONE', #2823, #1901, #10042 ) ;
#8194 = ORIENTED_EDGE ( 'NONE', *, *, #14246, .T. ) ;
#8195 = EDGE_CURVE ( 'NONE', #556, #5098, #4877, .T. ) ;
#8196 = ORIENTED_EDGE ( 'NONE', *, *, #3196, .F. ) ;
#8197 = CARTESIAN_POINT ( 'NONE',  ( 1.181102362204724310, -0.1240157480314955790, -0.02952755905511811330 ) ) ;
#8198 = AXIS2_PLACEMENT_3D ( 'NONE', #7347, #12155, #3531 ) ;
#8199 = DIRECTION ( 'NONE',  ( 0.000000000000000000, 1.000000000000000000, -0.000000000000000000 ) ) ;
#8200 = CARTESIAN_POINT ( 'NONE',  ( -1.922875500960418149, -2.878807188367765058, 0.1420686080738781387 ) ) ;
#8201 = VECTOR ( 'NONE', #15381, 39.37007874015748143 ) ;
#8202 = FACE_OUTER_BOUND ( 'NONE', #299, .T. ) ;
#8203 = DIRECTION ( 'NONE',  ( 0.000000000000000000, 0.000000000000000000, -1.000000000000000000 ) ) ;
#8204 = DIRECTION ( 'NONE',  ( 0.000000000000000000, 0.000000000000000000, -1.000000000000000000 ) ) ;
#8205 = DIRECTION ( 'NONE',  ( 1.000000000000000000, -8.673617379884051249E-15, 0.000000000000000000 ) ) ;
#8206 = CIRCLE ( 'NONE', #5674, 0.003937007874015735834 ) ;
#8207 = CARTESIAN_POINT ( 'NONE',  ( -0.1552072824047652788, 0.000000000000000000, -0.5870514566507987197 ) ) ;
#8208 = CARTESIAN_POINT ( 'NONE',  ( 0.000000000000000000, 0.5433070866141731514, -0.6692913385826770867 ) ) ;
#8209 = AXIS2_PLACEMENT_3D ( 'NONE', #6225, #6382, #12515 ) ;
#8210 = ORIENTED_EDGE ( 'NONE', *, *, #11828, .T. ) ;
#8211 = ORIENTED_EDGE ( 'NONE', *, *, #13916, .F. ) ;
#8212 = VERTEX_POINT ( 'NONE', #441 ) ;
#8213 = VERTEX_POINT ( 'NONE', #12566 ) ;
#8214 = EDGE_CURVE ( 'NONE', #6899, #8756, #1376, .T. ) ;
#8215 = B_SPLINE_CURVE_WITH_KNOTS ( 'NONE', 3,
 ( #5172, #4080, #13555, #12549 ),
 .UNSPECIFIED., .F., .F.,
 ( 4, 4 ),
 ( 0.0002461255424396399509, 0.0003583013531701036733 ),
 .UNSPECIFIED. ) ;
#8216 = DIRECTION ( 'NONE',  ( -0.8144815189573204606, 0.5801894994542525774, -0.000000000000000000 ) ) ;
#8217 = AXIS2_PLACEMENT_3D ( 'NONE', #14820, #2993, #12628 ) ;
#8218 = CARTESIAN_POINT ( 'NONE',  ( -0.02525249394761181279, 0.1725264476027946747, 0.03885236003517052172 ) ) ;
#8219 = ADVANCED_FACE ( 'NONE', ( #11236 ), #9385, .T. ) ;
#8220 = DIRECTION ( 'NONE',  ( -0.000000000000000000, -1.000000000000000000, -0.000000000000000000 ) ) ;
#8221 = CARTESIAN_POINT ( 'NONE',  ( 8.582170482213735190E-17, 0.5826771653543306728, 0.7007874015748031260 ) ) ;
#8222 = CARTESIAN_POINT ( 'NONE',  ( 0.06692913385832215123, -0.4921259842519685179, -0.5870514566507987197 ) ) ;
#8223 = ORIENTED_EDGE ( 'NONE', *, *, #10006, .T. ) ;
#8224 = DIRECTION ( 'NONE',  ( -0.000000000000000000, -1.000000000000000000, -0.000000000000000000 ) ) ;
#8225 = DIRECTION ( 'NONE',  ( 0.000000000000000000, -0.000000000000000000, -1.000000000000000000 ) ) ;
#8226 = CARTESIAN_POINT ( 'NONE',  ( -0.4815353412745217998, 1.041793866378536437, 0.3474236500605538125 ) ) ;
#8227 = AXIS2_PLACEMENT_3D ( 'NONE', #8859, #5236, #5163 ) ;
#8228 = ORIENTED_EDGE ( 'NONE', *, *, #5756, .T. ) ;
#8229 = ORIENTED_EDGE ( 'NONE', *, *, #404, .F. ) ;
#8230 = ORIENTED_EDGE ( 'NONE', *, *, #10576, .T. ) ;
#8231 = CARTESIAN_POINT ( 'NONE',  ( 0.000000000000000000, 0.07480314960629921850, -0.03937007874015751446 ) ) ;
#8232 = EDGE_CURVE ( 'NONE', #7004, #2439, #5337, .T. ) ;
#8233 = CARTESIAN_POINT ( 'NONE',  ( -1.925888590729081473, -2.947122644516800172, 0.02949560467575229258 ) ) ;
#8234 = DIRECTION ( 'NONE',  ( 0.8660254037844385966, -0.000000000000000000, -0.5000000000000001110 ) ) ;
#8235 = DIRECTION ( 'NONE',  ( 0.000000000000000000, -0.000000000000000000, -1.000000000000000000 ) ) ;
#8236 = CARTESIAN_POINT ( 'NONE',  ( -1.923270046725593430, -2.877647921889221028, 0.1430015488209055441 ) ) ;
#8237 = ORIENTED_EDGE ( 'NONE', *, *, #6739, .F. ) ;
#8238 = CARTESIAN_POINT ( 'NONE',  ( 0.000000000000000000, 0.07874015748031495954, 0.000000000000000000 ) ) ;
#8239 = LINE ( 'NONE', #13013, #5089 ) ;
#8240 = CARTESIAN_POINT ( 'NONE',  ( 0.4342073824196633347, -0.003937007874015747977, 0.4299076816772810505 ) ) ;
#8241 = LINE ( 'NONE', #4630, #14857 ) ;
#8242 = VERTEX_POINT ( 'NONE', #7776 ) ;
#8243 = ORIENTED_EDGE ( 'NONE', *, *, #11168, .T. ) ;
#8244 = ORIENTED_EDGE ( 'NONE', *, *, #9065, .T. ) ;
#8245 = ORIENTED_EDGE ( 'NONE', *, *, #12054, .T. ) ;
#8246 = VERTEX_POINT ( 'NONE', #1827 ) ;
#8247 = DIRECTION ( 'NONE',  ( 0.000000000000000000, 0.000000000000000000, 1.000000000000000000 ) ) ;
#8248 = DIRECTION ( 'NONE',  ( 0.8660254037844405950, 1.502314598737171929E-14, 0.4999999999999967804 ) ) ;
#8249 = DIRECTION ( 'NONE',  ( -0.5000000000000000000, 0.000000000000000000, 0.8660254037844385966 ) ) ;
#8250 = CARTESIAN_POINT ( 'NONE',  ( 0.000000000000000000, 0.1692468441617604180, -0.03937007874015747977 ) ) ;
#8251 = CONTEXT_DEPENDENT_SHAPE_REPRESENTATION ( #97, #453 ) ;
#8252 = CARTESIAN_POINT ( 'NONE',  ( 0.05905511811023622659, 1.043307086614173151, -0.8267716535433072833 ) ) ;
#8253 = EDGE_CURVE ( 'NONE', #13241, #6904, #7539, .T. ) ;
#8254 = CARTESIAN_POINT ( 'NONE',  ( -1.190198933766853706, 0.3259758027579612860, 0.05905511811023622659 ) ) ;
#8255 = EDGE_LOOP ( 'NONE', ( #7276, #10711, #15237, #384 ) ) ;
#8256 = CARTESIAN_POINT ( 'NONE',  ( -1.180847381051866707, 0.3433074774306728028, 0.05905511811023622659 ) ) ;
#8257 = CARTESIAN_POINT ( 'NONE',  ( 0.000000000000000000, -0.4921259842519685179, 0.1768186671464649640 ) ) ;
#8258 = EDGE_CURVE ( 'NONE', #2728, #15156, #12649, .T. ) ;
#8259 = DIRECTION ( 'NONE',  ( -1.000000000000000000, 0.000000000000000000, 0.000000000000000000 ) ) ;
#8260 = ORIENTED_EDGE ( 'NONE', *, *, #5282, .T. ) ;
#8261 = DIRECTION ( 'NONE',  ( -1.000000000000000000, 0.000000000000000000, 0.000000000000000000 ) ) ;
#8262 = ORIENTED_EDGE ( 'NONE', *, *, #10419, .F. ) ;
#8263 = ORIENTED_EDGE ( 'NONE', *, *, #8166, .F. ) ;
#8264 = VERTEX_POINT ( 'NONE', #15067 ) ;
#8265 = DIRECTION ( 'NONE',  ( 0.4999999999999966693, 0.000000000000000000, -0.8660254037844405950 ) ) ;
#8266 = CARTESIAN_POINT ( 'NONE',  ( -1.906686051247057145, -2.925149623272649713, -0.09038834661822293948 ) ) ;
#8267 = EDGE_CURVE ( 'NONE', #14387, #6881, #11894, .T. ) ;
#8268 = EDGE_CURVE ( 'NONE', #14788, #14790, #12140, .T. ) ;
#8269 = CARTESIAN_POINT ( 'NONE',  ( 0.000000000000000000, 0.000000000000000000, -0.5511811023622046335 ) ) ;
#8270 = DIRECTION ( 'NONE',  ( 1.000000000000000000, -0.000000000000000000, 1.224646799147353207E-16 ) ) ;
#8271 = CARTESIAN_POINT ( 'NONE',  ( 2.025006518275150778E-17, 0.03937007874015749365, 0.1653543307086614012 ) ) ;
#8272 = EDGE_CURVE ( 'NONE', #12093, #4326, #15240, .T. ) ;
#8273 = LINE ( 'NONE', #919, #5823 ) ;
#8274 = DIRECTION ( 'NONE',  ( 0.000000000000000000, 0.000000000000000000, 1.000000000000000000 ) ) ;
#8275 = ORIENTED_EDGE ( 'NONE', *, *, #12396, .F. ) ;
#8276 = ORIENTED_EDGE ( 'NONE', *, *, #4740, .T. ) ;
#8277 = ORIENTED_EDGE ( 'NONE', *, *, #4923, .T. ) ;
#8278 = ORIENTED_EDGE ( 'NONE', *, *, #15304, .F. ) ;
#8279 = CARTESIAN_POINT ( 'NONE',  ( -0.1062992125983150127, -0.09842519685039370636, -0.2482618547482104143 ) ) ;
#8280 = EDGE_CURVE ( 'NONE', #11605, #10010, #5352, .T. ) ;
#8281 = CARTESIAN_POINT ( 'NONE',  ( 1.181102362204724310, 4.044111181948214319E-16, 0.02952755905511811330 ) ) ;
#8282 = CARTESIAN_POINT ( 'NONE',  ( -0.01782267696647955174, -0.1622289191103822303, -0.03095755538600572856 ) ) ;
#8283 = DIRECTION ( 'NONE',  ( 0.5984233124757279976, 0.8011800915434538206, 0.000000000000000000 ) ) ;
#8284 = CARTESIAN_POINT ( 'NONE',  ( 0.3137366569588399545, -0.2952755905511811330, 0.2947875711430715251 ) ) ;
#8285 = ORIENTED_EDGE ( 'NONE', *, *, #1800, .T. ) ;
#8286 = CARTESIAN_POINT ( 'NONE',  ( 8.100026073100603114E-17, 0.3622047244094487306, 0.6614173228346456046 ) ) ;
#8287 = EDGE_CURVE ( 'NONE', #12429, #7254, #8016, .T. ) ;
#8288 = LINE ( 'NONE', #5764, #9863 ) ;
#8289 = CARTESIAN_POINT ( 'NONE',  ( 0.6523822077042866763, 1.190944881889763884, 0.4448440199085238467 ) ) ;
#8290 = VERTEX_POINT ( 'NONE', #15150 ) ;
#8291 = EDGE_LOOP ( 'NONE', ( #12029, #8190, #1779, #2330 ) ) ;
#8292 = EDGE_CURVE ( 'NONE', #12093, #13620, #14136, .T. ) ;
#8293 = ORIENTED_EDGE ( 'NONE', *, *, #5473, .F. ) ;
#8294 = DIRECTION ( 'NONE',  ( -1.000000000000000000, 0.000000000000000000, 0.000000000000000000 ) ) ;
#8295 = CARTESIAN_POINT ( 'NONE',  ( -1.938865708396552590, -2.947839766983606946, 0.02498451593668036402 ) ) ;
#8296 = DIRECTION ( 'NONE',  ( 1.000000000000000000, 0.000000000000000000, 0.000000000000000000 ) ) ;
#8297 = DIRECTION ( 'NONE',  ( -1.000000000000000000, 0.000000000000000000, 0.000000000000000000 ) ) ;
#8298 = FACE_OUTER_BOUND ( 'NONE', #3391, .T. ) ;
#8299 = CARTESIAN_POINT ( 'NONE',  ( -0.4788739157331332597, -0.1023622047244094474, 0.3446689608323532106 ) ) ;
#8300 = CARTESIAN_POINT ( 'NONE',  ( -1.912441115949275794, -2.839038486429707575, 0.1647378018180373216 ) ) ;
#8301 = VERTEX_POINT ( 'NONE', #10525 ) ;
#8302 = CARTESIAN_POINT ( 'NONE',  ( -1.991669579775100729, -2.812944829929203916, -0.1541819158628824904 ) ) ;
#8303 = DIRECTION ( 'NONE',  ( 0.000000000000000000, -1.000000000000000000, 0.000000000000000000 ) ) ;
#8304 = CARTESIAN_POINT ( 'NONE',  ( 0.1028896637646825735, -0.09842519685039372024, -0.2462933508111075642 ) ) ;
#8305 = SPHERICAL_SURFACE ( 'NONE', #8102, 0.003937007874015747977 ) ;
#8306 = ORIENTED_EDGE ( 'NONE', *, *, #1301, .T. ) ;
#8307 = EDGE_CURVE ( 'NONE', #14774, #2262, #3246, .T. ) ;
#8308 = ORIENTED_EDGE ( 'NONE', *, *, #10390, .F. ) ;
#8309 = ORIENTED_EDGE ( 'NONE', *, *, #3982, .F. ) ;
#8310 = VECTOR ( 'NONE', #5575, 39.37007874015748143 ) ;
#8311 = DIRECTION ( 'NONE',  ( 0.000000000000000000, 0.000000000000000000, -1.000000000000000000 ) ) ;
#8312 = CARTESIAN_POINT ( 'NONE',  ( 0.000000000000000000, -0.1023622047244094474, 0.000000000000000000 ) ) ;
#8313 = FACE_OUTER_BOUND ( 'NONE', #15075, .T. ) ;
#8314 = CONTEXT_DEPENDENT_SHAPE_REPRESENTATION ( #3798, #15167 ) ;
#8315 = LINE ( 'NONE', #5796, #8201 ) ;
#8316 = DIRECTION ( 'NONE',  ( 0.000000000000000000, 0.000000000000000000, -1.000000000000000000 ) ) ;
#8317 = ORIENTED_EDGE ( 'NONE', *, *, #3796, .T. ) ;
#8318 = CARTESIAN_POINT ( 'NONE',  ( -1.607606114292111643, 0.09732815221480063672, -0.07874015748031495954 ) ) ;
#8319 = FACE_OUTER_BOUND ( 'NONE', #3051, .T. ) ;
#8320 = CARTESIAN_POINT ( 'NONE',  ( 0.1062992125984795477, -0.09842519685039370636, -0.2482618547481155458 ) ) ;
#8321 = DIRECTION ( 'NONE',  ( 0.8660254037844384856, 0.000000000000000000, 0.5000000000000004441 ) ) ;
#8322 = VERTEX_POINT ( 'NONE', #6754 ) ;
#8323 = VERTEX_POINT ( 'NONE', #4562 ) ;
#8324 = EDGE_LOOP ( 'NONE', ( #14897, #13493 ) ) ;
#8325 = EDGE_LOOP ( 'NONE', ( #3212, #12699, #9523, #15445 ) ) ;
#8326 = ORIENTED_EDGE ( 'NONE', *, *, #4043, .F. ) ;
#8327 = DIRECTION ( 'NONE',  ( -0.000000000000000000, -1.000000000000000000, -0.000000000000000000 ) ) ;
#8328 = AXIS2_PLACEMENT_3D ( 'NONE', #7287, #8397, #5879 ) ;
#8329 = TOROIDAL_SURFACE ( 'NONE', #11583, 0.1240157480314959815, 0.003937007874015747977 ) ;
#8330 = AXIS2_PLACEMENT_3D ( 'NONE', #13691, #8991, #4040 ) ;
#8331 = EDGE_CURVE ( 'NONE', #14773, #8390, #1051, .T. ) ;
#8332 = DIRECTION ( 'NONE',  ( -0.000000000000000000, 1.000000000000000000, 0.000000000000000000 ) ) ;
#8333 = DIRECTION ( 'NONE',  ( -0.8660254037844363761, 0.000000000000000000, 0.5000000000000038858 ) ) ;
#8334 = AXIS2_PLACEMENT_3D ( 'NONE', #14423, #13238, #11028 ) ;
#8335 = CARTESIAN_POINT ( 'NONE',  ( -0.6274225779320011798, 37.37889961492984270, 0.5668155242925447812 ) ) ;
#8336 = CARTESIAN_POINT ( 'NONE',  ( 6.846450609406462919E-17, 1.614173228346457156, -0.5590551181102362266 ) ) ;
#8337 = CARTESIAN_POINT ( 'NONE',  ( -1.395867684562290378, -0.02540710596904927759, 0.04030457392454530469 ) ) ;
#8338 = CARTESIAN_POINT ( 'NONE',  ( -1.961854477779698014, -2.757150671784349694, 0.1766817721349826786 ) ) ;
#8339 = DIRECTION ( 'NONE',  ( 0.000000000000000000, 2.212657494868377674E-16, -1.000000000000000000 ) ) ;
#8340 = AXIS2_PLACEMENT_3D ( 'NONE', #12949, #15458, #12074 ) ;
#8341 = AXIS2_PLACEMENT_3D ( 'NONE', #1535, #9936, #7645 ) ;
#8342 = ORIENTED_EDGE ( 'NONE', *, *, #10282, .F. ) ;
#8343 = EDGE_CURVE ( 'NONE', #3491, #7659, #9349, .T. ) ;
#8344 = AXIS2_PLACEMENT_3D ( 'NONE', #10272, #12779, #10341 ) ;
#8345 = ORIENTED_EDGE ( 'NONE', *, *, #14500, .F. ) ;
#8346 = VECTOR ( 'NONE', #8658, 39.37007874015748143 ) ;
#8347 = ORIENTED_EDGE ( 'NONE', *, *, #11951, .T. ) ;
#8348 = EDGE_CURVE ( 'NONE', #2464, #1302, #3637, .T. ) ;
#8349 = ORIENTED_EDGE ( 'NONE', *, *, #12271, .F. ) ;
#8350 = ADVANCED_FACE ( 'NONE', ( #14130, #4414 ), #891, .T. ) ;
#8351 = CARTESIAN_POINT ( 'NONE',  ( -0.5511811023622046335, 0.3543307086614172485, 0.000000000000000000 ) ) ;
#8352 = VECTOR ( 'NONE', #147, 39.37007874015748143 ) ;
#8353 = CARTESIAN_POINT ( 'NONE',  ( 0.000000000000000000, 2.448818897637795367, -0.03937007874015747977 ) ) ;
#8354 = VECTOR ( 'NONE', #14810, 39.37007874015748143 ) ;
#8355 = DIRECTION ( 'NONE',  ( -0.8660254037844398178, 0.000000000000000000, 0.4999999999999979461 ) ) ;
#8356 = VECTOR ( 'NONE', #14029, 39.37007874015748143 ) ;
#8357 = FACE_OUTER_BOUND ( 'NONE', #15090, .T. ) ;
#8358 = DIRECTION ( 'NONE',  ( -3.942553354492736135E-16, 0.000000000000000000, 1.000000000000000000 ) ) ;
#8359 = ORIENTED_EDGE ( 'NONE', *, *, #10779, .F. ) ;
#8360 = DIRECTION ( 'NONE',  ( -1.000000000000000000, 0.000000000000000000, -3.973232667114494807E-16 ) ) ;
#8361 = DIRECTION ( 'NONE',  ( -0.4999999999999966693, 0.000000000000000000, -0.8660254037844405950 ) ) ;
#8362 = ADVANCED_BREP_SHAPE_REPRESENTATION ( '', ( #9119, #11481 ), #5701 ) ;
#8363 = EDGE_LOOP ( 'NONE', ( #1693, #3265, #14492 ) ) ;
#8364 = ORIENTED_EDGE ( 'NONE', *, *, #13314, .T. ) ;
#8365 = TOROIDAL_SURFACE ( 'NONE', #5097, 0.2303149606299203511, 0.01968503937007873988 ) ;
#8366 = AXIS2_PLACEMENT_3D ( 'NONE', #7737, #5287, #13533 ) ;
#8367 = AXIS2_PLACEMENT_3D ( 'NONE', #4675, #9462, #3500 ) ;
#8368 = EDGE_CURVE ( 'NONE', #11513, #10081, #144, .T. ) ;
#8369 = VECTOR ( 'NONE', #7751, 39.37007874015748143 ) ;
#8370 = ORIENTED_EDGE ( 'NONE', *, *, #15357, .F. ) ;
#8371 = AXIS2_PLACEMENT_3D ( 'NONE', #1190, #9411, #14185 ) ;
#8372 = CARTESIAN_POINT ( 'NONE',  ( -1.985311755390524624, -2.772329397582317778, 0.1771653543307079026 ) ) ;
#8373 = CARTESIAN_POINT ( 'NONE',  ( -1.900068616880432160, -2.943488425837897271, 0.04725664440068118310 ) ) ;
#8374 = EDGE_CURVE ( 'NONE', #6704, #5049, #4651, .T. ) ;
#8375 = CARTESIAN_POINT ( 'NONE',  ( -1.607606113623927691, 0.09732815316532632266, 0.07192616626583318851 ) ) ;
#8376 = CARTESIAN_POINT ( 'NONE',  ( -1.930187871534237765, -2.935355666847295986, -0.06964585819737736938 ) ) ;
#8377 = CARTESIAN_POINT ( 'NONE',  ( -0.1259842519685039353, 2.440944881889763884, -0.04724409448818898266 ) ) ;
#8378 = CARTESIAN_POINT ( 'NONE',  ( -0.03213667549430108267, -0.1820030000337380938, -0.02170016096604327968 ) ) ;
#8379 = DIRECTION ( 'NONE',  ( -0.000000000000000000, 0.000000000000000000, 1.000000000000000000 ) ) ;
#8380 = CIRCLE ( 'NONE', #12879, 0.5590551181102362266 ) ;
#8381 = CARTESIAN_POINT ( 'NONE',  ( 0.4749369078591172411, -0.4881889763779528324, 0.3514880584999470203 ) ) ;
#8382 = VECTOR ( 'NONE', #15007, 39.37007874015748854 ) ;
#8383 = CARTESIAN_POINT ( 'NONE',  ( -1.942131557808294717, -2.755773022703220665, 0.1769289245135293731 ) ) ;
#8384 = AXIS2_PLACEMENT_3D ( 'NONE', #10172, #12450, #12289 ) ;
#8385 = ORIENTED_EDGE ( 'NONE', *, *, #3363, .T. ) ;
#8386 = CARTESIAN_POINT ( 'NONE',  ( -1.945338968710944361, -2.932170493076832862, -0.04030640840855362339 ) ) ;
#8387 = DIRECTION ( 'NONE',  ( 0.000000000000000000, 0.000000000000000000, -1.000000000000000000 ) ) ;
#8388 = AXIS2_PLACEMENT_3D ( 'NONE', #12229, #3821, #9791 ) ;
#8389 = CARTESIAN_POINT ( 'NONE',  ( -0.06692913385815749128, -0.4921259842519685179, -0.2377126739438355507 ) ) ;
#8390 = VERTEX_POINT ( 'NONE', #6918 ) ;
#8392 = ORIENTED_EDGE ( 'NONE', *, *, #4923, .F. ) ;
#8391 = AXIS2_PLACEMENT_3D ( 'NONE', #10862, #9392, #8358 ) ;
#8393 = TOROIDAL_SURFACE ( 'NONE', #3136, 0.6614173228346456046, 0.007874015748031495954 ) ;
#8394 = CARTESIAN_POINT ( 'NONE',  ( -0.2359202325321149429, -0.4921259842519685179, 0.06286251073437550130 ) ) ;
#8395 = VECTOR ( 'NONE', #9490, 39.37007874015748143 ) ;
#8396 = EDGE_CURVE ( 'NONE', #517, #11768, #7362, .T. ) ;
#8397 = DIRECTION ( 'NONE',  ( -0.8660254037844352659, 0.000000000000000000, 0.5000000000000058842 ) ) ;
#8398 = AXIS2_PLACEMENT_3D ( 'NONE', #4893, #9689, #14466 ) ;
#8399 = APPLICATION_CONTEXT ( 'automotive_design' ) ;
#8400 = LINE ( 'NONE', #3772, #8877 ) ;
#8401 = CYLINDRICAL_SURFACE ( 'NONE', #11116, 0.003937007874015750579 ) ;
#8402 = LINE ( 'NONE', #8252, #8696 ) ;
#8403 = DIRECTION ( 'NONE',  ( 0.000000000000000000, 1.000000000000000000, 0.000000000000000000 ) ) ;
#8404 = EDGE_CURVE ( 'NONE', #15326, #1672, #2130, .T. ) ;
#8405 = EDGE_LOOP ( 'NONE', ( #969, #10565, #1917, #7163 ) ) ;
#8406 = CARTESIAN_POINT ( 'NONE',  ( -0.1618514667033796040, -0.1023622047244094474, 0.2122517380126066888 ) ) ;
#8407 = EDGE_CURVE ( 'NONE', #5098, #11032, #629, .T. ) ;
#8408 = DIRECTION ( 'NONE',  ( 0.8660254037844363761, 0.000000000000000000, -0.5000000000000038858 ) ) ;
#8409 = VECTOR ( 'NONE', #1748, 39.37007874015748143 ) ;
#8410 = AXIS2_PLACEMENT_3D ( 'NONE', #467, #5212, #12349 ) ;
#8411 = FACE_OUTER_BOUND ( 'NONE', #4685, .T. ) ;
#8412 = AXIS2_PLACEMENT_3D ( 'NONE', #5606, #1010, #11659 ) ;
#8413 = FACE_OUTER_BOUND ( 'NONE', #10295, .T. ) ;
#8414 = VECTOR ( 'NONE', #8015, 39.37007874015748143 ) ;
#8415 = ORIENTED_EDGE ( 'NONE', *, *, #14962, .F. ) ;
#8416 = ORIENTED_EDGE ( 'NONE', *, *, #8232, .F. ) ;
#8417 = ORIENTED_EDGE ( 'NONE', *, *, #8741, .F. ) ;
#8418 = ORIENTED_EDGE ( 'NONE', *, *, #5019, .T. ) ;
#8419 = DIRECTION ( 'NONE',  ( 0.000000000000000000, -0.000000000000000000, 1.000000000000000000 ) ) ;
#8420 = AXIS2_PLACEMENT_3D ( 'NONE', #4811, #5677, #3629 ) ;
#8421 = FACE_OUTER_BOUND ( 'NONE', #8004, .T. ) ;
#8422 = DIRECTION ( 'NONE',  ( -0.8660254037844385966, 0.000000000000000000, -0.5000000000000001110 ) ) ;
#8423 = DIRECTION ( 'NONE',  ( 0.2084205441254162738, 0.9706086590632808653, -0.1203316572554590097 ) ) ;
#8424 = CARTESIAN_POINT ( 'NONE',  ( 0.4307978335858662633, -0.09448818897637796532, 0.4279391777402732910 ) ) ;
#8425 = FACE_OUTER_BOUND ( 'NONE', #4795, .T. ) ;
#8426 = DIRECTION ( 'NONE',  ( 0.000000000000000000, 0.000000000000000000, 1.000000000000000000 ) ) ;
#8427 = LINE ( 'NONE', #4673, #3822 ) ;
#8428 = DIRECTION ( 'NONE',  ( 1.000000000000000000, 0.000000000000000000, 0.000000000000000000 ) ) ;
#8429 = FACE_OUTER_BOUND ( 'NONE', #5005, .T. ) ;
#8430 = CARTESIAN_POINT ( 'NONE',  ( -0.06692913385815749128, -0.4921259842519685179, -0.2377126739438355507 ) ) ;
#8431=STYLED_ITEM('',(#15533),#9613);
#8432 = ORIENTED_EDGE ( 'NONE', *, *, #12766, .F. ) ;
#8433 = ORIENTED_EDGE ( 'NONE', *, *, #2596, .T. ) ;
#8434 = CIRCLE ( 'NONE', #10697, 0.03937007874015750752 ) ;
#8435 = ORIENTED_EDGE ( 'NONE', *, *, #3600, .T. ) ;
#8436 = TOROIDAL_SURFACE ( 'NONE', #4429, 0.5984251968503937480, 0.007874015748031495954 ) ;
#8437 = DIRECTION ( 'NONE',  ( -1.000000000000000000, -0.000000000000000000, -0.000000000000000000 ) ) ;
#8438 = VECTOR ( 'NONE', #2974, 39.37007874015748143 ) ;
#8439 = DIRECTION ( 'NONE',  ( -0.000000000000000000, 1.000000000000000000, 0.000000000000000000 ) ) ;
#8440 = AXIS2_PLACEMENT_3D ( 'NONE', #15260, #2013, #12822 ) ;
#8441 = DIRECTION ( 'NONE',  ( 0.000000000000000000, 1.000000000000000000, 0.000000000000000000 ) ) ;
#8442 = EDGE_CURVE ( 'NONE', #2963, #10145, #8623, .T. ) ;
#8443 = DIRECTION ( 'NONE',  ( 0.000000000000000000, 0.000000000000000000, 1.000000000000000000 ) ) ;
#8444 = DIRECTION ( 'NONE',  ( -0.4999999999999986122, 2.168404344971006501E-15, 0.8660254037844395958 ) ) ;
#8445 = AXIS2_PLACEMENT_3D ( 'NONE', #7527, #12175, #3783 ) ;
#8446 = FACE_OUTER_BOUND ( 'NONE', #14992, .T. ) ;
#8447 = EDGE_CURVE ( 'NONE', #1873, #15252, #8926, .T. ) ;
#8448 = DIRECTION ( 'NONE',  ( -1.000000000000000000, -6.505213034913066047E-15, -0.000000000000000000 ) ) ;
#8449 = CARTESIAN_POINT ( 'NONE',  ( 0.05905511811023625435, 2.637795275590551825, 0.03937007874015747977 ) ) ;
#8450 = DIRECTION ( 'NONE',  ( -1.000000000000000000, 0.000000000000000000, 1.669238443041289401E-16 ) ) ;
#8451 = VECTOR ( 'NONE', #15299, 39.37007874015748854 ) ;
#8452 = ORIENTED_EDGE ( 'NONE', *, *, #4288, .T. ) ;
#8453 = EDGE_CURVE ( 'NONE', #8061, #11513, #4128, .T. ) ;
#8454 = ORIENTED_EDGE ( 'NONE', *, *, #11623, .T. ) ;
#8455 = CIRCLE ( 'NONE', #8702, 0.007874015748031482076 ) ;
#8456 = ORIENTED_EDGE ( 'NONE', *, *, #2072, .F. ) ;
#8457 = VECTOR ( 'NONE', #5969, 39.37007874015748854 ) ;
#8458 = PLANE ( 'NONE',  #2634 ) ;
#8459 = CARTESIAN_POINT ( 'NONE',  ( -1.595687817112648954, 0.1142625427334059557, 0.07194693897042922504 ) ) ;
#8460 = EDGE_CURVE ( 'NONE', #11277, #113, #1215, .T. ) ;
#8461 = FACE_OUTER_BOUND ( 'NONE', #15108, .T. ) ;
#8462 = DIRECTION ( 'NONE',  ( 0.000000000000000000, 1.000000000000000000, 0.000000000000000000 ) ) ;
#8463 = FACE_OUTER_BOUND ( 'NONE', #13818, .T. ) ;
#8465 = AXIS2_PLACEMENT_3D ( 'NONE', #9971, #8781, #6418 ) ;
#8464 = DIRECTION ( 'NONE',  ( -1.000000000000000000, 0.000000000000000000, 0.000000000000000000 ) ) ;
#8466 = CARTESIAN_POINT ( 'NONE',  ( -1.934032282416884740, -2.845555853951683201, 0.1617933121749894620 ) ) ;
#8467 = ADVANCED_FACE ( 'NONE', ( #5968 ), #14394, .F. ) ;
#8468 = ORIENTED_EDGE ( 'NONE', *, *, #10836, .F. ) ;
#8469 = CARTESIAN_POINT ( 'NONE',  ( 0.1062992125984795477, -0.1023622047244094474, -0.2472069366676780122 ) ) ;
#8470 = CIRCLE ( 'NONE', #5194, 0.05905511811023627516 ) ;
#8471 = CARTESIAN_POINT ( 'NONE',  ( -0.01783696211247718169, 0.1513009196653194166, -0.03097470637416573774 ) ) ;
#8472 = ORIENTED_EDGE ( 'NONE', *, *, #5832, .F. ) ;
#8473 = EDGE_CURVE ( 'NONE', #10209, #6217, #8486, .T. ) ;
#8474 = ORIENTED_EDGE ( 'NONE', *, *, #10832, .T. ) ;
#8475 = ORIENTED_EDGE ( 'NONE', *, *, #15420, .F. ) ;
#8476 = AXIS2_PLACEMENT_3D ( 'NONE', #4775, #8235, #14097 ) ;
#8477 = DIRECTION ( 'NONE',  ( 0.000000000000000000, 1.000000000000000000, 0.000000000000000000 ) ) ;
#8478 = CARTESIAN_POINT ( 'NONE',  ( -1.395776408008654990, -0.02488039011573578430, 0.06612399333097303267 ) ) ;
#8479 = PLANE ( 'NONE',  #12143 ) ;
#8480 = ITEM_DEFINED_TRANSFORMATION ( 'NONE', 'NONE', #14127,  #11481 ) ;
#8481 = DIRECTION ( 'NONE',  ( 1.224646799147353947E-16, 0.000000000000000000, -1.000000000000000000 ) ) ;
#8482 = CARTESIAN_POINT ( 'NONE',  ( 6.750021727583836750E-17, 0.000000000000000000, 0.5511811023622046335 ) ) ;
#8483 = ADVANCED_FACE ( 'NONE', ( #6194 ), #1510, .F. ) ;
#8484 = ORIENTED_EDGE ( 'NONE', *, *, #13252, .T. ) ;
#8485 = CARTESIAN_POINT ( 'NONE',  ( -1.593720380427063876, 0.1169877005562839495, -0.06604764719695267738 ) ) ;
#8486 = LINE ( 'NONE', #8548, #6878 ) ;
#8487 = CARTESIAN_POINT ( 'NONE',  ( -0.03549374849269339854, -0.1824859222442999918, 0.04671604978335693048 ) ) ;
#8488 = EDGE_CURVE ( 'NONE', #6775, #10534, #1350, .T. ) ;
#8489 = DIRECTION ( 'NONE',  ( 0.8660254037844383745, 0.000000000000000000, 0.5000000000000004441 ) ) ;
#8490 = EDGE_CURVE ( 'NONE', #11452, #3552, #2872, .T. ) ;
#8491 = EDGE_LOOP ( 'NONE', ( #1906, #7607, #5787 ) ) ;
#8492 = EDGE_LOOP ( 'NONE', ( #8161, #14137, #1853 ) ) ;
#8493 = ORIENTED_EDGE ( 'NONE', *, *, #10585, .F. ) ;
#8494 = VERTEX_POINT ( 'NONE', #13191 ) ;
#8495 = EDGE_CURVE ( 'NONE', #12240, #5035, #1139, .T. ) ;
#8496 = DIRECTION ( 'NONE',  ( 0.000000000000000000, -0.000000000000000000, -1.000000000000000000 ) ) ;
#8497 = CARTESIAN_POINT ( 'NONE',  ( 1.181102362204724310, 0.1279527559055117225, 0.02559055118110236185 ) ) ;
#8498 = DIRECTION ( 'NONE',  ( -0.8660254037844385966, 0.000000000000000000, -0.5000000000000000000 ) ) ;
#8499 = DIRECTION ( 'NONE',  ( 0.4932581959314706888, 0.8219459448134281976, 0.2847827522010268897 ) ) ;
#8500 = DIRECTION ( 'NONE',  ( 1.000000000000000000, -0.000000000000000000, -0.000000000000000000 ) ) ;
#8501 = DIRECTION ( 'NONE',  ( 0.5000000000000041078, -0.000000000000000000, 0.8660254037844363761 ) ) ;
#8502 = CARTESIAN_POINT ( 'NONE',  ( 0.000000000000000000, 0.007874015748031480341, 0.000000000000000000 ) ) ;
#8503 = DIRECTION ( 'NONE',  ( 0.000000000000000000, 1.000000000000000000, -8.673617379884035472E-15 ) ) ;
#8504 = PLANE ( 'NONE',  #1835 ) ;
#8505 = EDGE_LOOP ( 'NONE', ( #8364, #2628, #5874, #3449 ) ) ;
#8506 = ORIENTED_EDGE ( 'NONE', *, *, #8267, .T. ) ;
#8507 = ORIENTED_EDGE ( 'NONE', *, *, #2012, .F. ) ;
#8508 = EDGE_CURVE ( 'NONE', #1093, #13132, #6116, .T. ) ;
#8509 = CARTESIAN_POINT ( 'NONE',  ( -1.293236445124221312, 0.1355266887446167634, -0.03937007874015747977 ) ) ;
#8510 = CARTESIAN_POINT ( 'NONE',  ( -1.315994971760645248E-15, -0.09842519685039370636, 0.4279391777402719588 ) ) ;
#8511 = DIRECTION ( 'NONE',  ( -0.000000000000000000, -1.000000000000000000, 0.000000000000000000 ) ) ;
#8512 = CARTESIAN_POINT ( 'NONE',  ( 0.06299212598430639631, -0.4881889763779528324, -0.5909884645248143498 ) ) ;
#8513 = DIRECTION ( 'NONE',  ( -0.000000000000000000, -1.000000000000000000, -0.000000000000000000 ) ) ;
#8514 = CARTESIAN_POINT ( 'NONE',  ( -0.05905511811023622659, 1.190944881889763884, -0.8267716535433072833 ) ) ;
#8515 = DIRECTION ( 'NONE',  ( 0.000000000000000000, 0.000000000000000000, 1.000000000000000000 ) ) ;
#8516 = DIRECTION ( 'NONE',  ( -0.000000000000000000, -1.000000000000000000, -0.000000000000000000 ) ) ;
#8517 = CARTESIAN_POINT ( 'NONE',  ( -1.224409448818897461, 5.303588500244450842E-18, 0.02952755905511811330 ) ) ;
#8518 = EDGE_LOOP ( 'NONE', ( #9871, #1494, #2025, #12646 ) ) ;
#8519 = VERTEX_POINT ( 'NONE', #13262 ) ;
#8520 = ORIENTED_EDGE ( 'NONE', *, *, #13005, .F. ) ;
#8521 = ORIENTED_EDGE ( 'NONE', *, *, #15255, .T. ) ;
#8522 = DIRECTION ( 'NONE',  ( 1.000000000000000000, 0.000000000000000000, 0.000000000000000000 ) ) ;
#8523 = CARTESIAN_POINT ( 'NONE',  ( -1.584743043511021909, 0.1295304748375773751, -0.05905511811023622659 ) ) ;
#8524 = ADVANCED_FACE ( 'NONE', ( #2456 ), #34, .F. ) ;
#8525 = DIRECTION ( 'NONE',  ( -0.000000000000000000, -0.000000000000000000, -1.000000000000000000 ) ) ;
#8526 = FACE_OUTER_BOUND ( 'NONE', #15428, .T. ) ;
#8527 = CARTESIAN_POINT ( 'NONE',  ( -2.054794062199362781, -2.568933014740236498, 0.1522411129244188310 ) ) ;
#8528 = FACE_OUTER_BOUND ( 'NONE', #6279, .T. ) ;
#8529 = CARTESIAN_POINT ( 'NONE',  ( -1.926804229133072699, -2.867234193721032831, 0.1501075262831944590 ) ) ;
#8530 = EDGE_LOOP ( 'NONE', ( #5991, #14864, #14568, #11377 ) ) ;
#8531 = CARTESIAN_POINT ( 'NONE',  ( -1.955247660674698906, -2.907829365248872033, -0.09169626363195912400 ) ) ;
#8532 = CARTESIAN_POINT ( 'NONE',  ( -0.09842519685028340570, -0.4881889763779528324, -0.5870514566507987197 ) ) ;
#8533 = ORIENTED_EDGE ( 'NONE', *, *, #11823, .F. ) ;
#8534 = EDGE_LOOP ( 'NONE', ( #10147, #6741 ) ) ;
#8535 = EDGE_CURVE ( 'NONE', #8145, #12044, #10817, .T. ) ;
#8536 = EDGE_LOOP ( 'NONE', ( #11978, #6643, #11776, #5214 ) ) ;
#8537 = ADVANCED_FACE ( 'NONE', ( #14449 ), #2633, .T. ) ;
#8538 = DIRECTION ( 'NONE',  ( -0.000000000000000000, -0.000000000000000000, -1.000000000000000000 ) ) ;
#8539 = CARTESIAN_POINT ( 'NONE',  ( 0.05175539059627461136, 0.06736074103232447818, -0.07475334604056278753 ) ) ;
#8540 = EDGE_CURVE ( 'NONE', #8021, #2098, #1154, .T. ) ;
#8541 = CARTESIAN_POINT ( 'NONE',  ( -1.602377441323804996, 0.1047452084010624673, -0.05343540472197173818 ) ) ;
#8542 = DIRECTION ( 'NONE',  ( -0.5801894994542525774, -0.8144815189573204606, 0.000000000000000000 ) ) ;
#8543 = DIRECTION ( 'NONE',  ( -1.349229370204184172E-15, -1.000000000000000000, 0.000000000000000000 ) ) ;
#8544 = DIRECTION ( 'NONE',  ( -0.5000000000000001110, 0.000000000000000000, 0.8660254037844385966 ) ) ;
#8545 = ORIENTED_EDGE ( 'NONE', *, *, #14101, .F. ) ;
#8546 = CARTESIAN_POINT ( 'NONE',  ( -1.596293587998522945, 0.1133155780025432574, -0.04477369844328129428 ) ) ;
#8547 = PLANE ( 'NONE',  #347 ) ;
#8548 = CARTESIAN_POINT ( 'NONE',  ( 0.1023622047244638067, -0.4881889763779528324, -0.2472069366676780122 ) ) ;
#8549 = CARTESIAN_POINT ( 'NONE',  ( 0.09948011493088554369, -0.4921259842519685179, -0.2443248468740996937 ) ) ;
#8550 = CARTESIAN_POINT ( 'NONE',  ( -0.1574803149606299191, -0.09448818897637796532, -0.5909884645248143498 ) ) ;
#8551 = VERTEX_POINT ( 'NONE', #9750 ) ;
#8552 = EDGE_CURVE ( 'NONE', #7182, #14789, #11653, .T. ) ;
#8553 = EDGE_LOOP ( 'NONE', ( #9283, #10448, #302, #1221 ) ) ;
#8554 = ORIENTED_EDGE ( 'NONE', *, *, #6739, .T. ) ;
#8555 = EDGE_CURVE ( 'NONE', #13444, #10362, #5124, .T. ) ;
#8556 = VERTEX_POINT ( 'NONE', #4729 ) ;
#8557 = CARTESIAN_POINT ( 'NONE',  ( -2.755905511811024056, -2.772329397582842248, 0.000000000000000000 ) ) ;
#8558 = ADVANCED_FACE ( 'NONE', ( #8319 ), #7152, .F. ) ;
#8559 = DIRECTION ( 'NONE',  ( 0.7402970580929170152, 0.6722799013647308142, 0.000000000000000000 ) ) ;
#8560 = CARTESIAN_POINT ( 'NONE',  ( -1.100415514366356762, -0.04998955061627542718, 0.05905511811023622659 ) ) ;
#8561 = CARTESIAN_POINT ( 'NONE',  ( 0.6569501369871398877, 37.37889961492984980, 0.5156722917855650623 ) ) ;
#8562 = EDGE_CURVE ( 'NONE', #5281, #11243, #3649, .T. ) ;
#8563 = FACE_OUTER_BOUND ( 'NONE', #15292, .T. ) ;
#8564 = CARTESIAN_POINT ( 'NONE',  ( 0.4783464566929142014, -0.09842519685039370636, 0.3534565624369548908 ) ) ;
#8565 = DIRECTION ( 'NONE',  ( -0.000000000000000000, -0.000000000000000000, -1.000000000000000000 ) ) ;
#8566 = DIRECTION ( 'NONE',  ( 0.000000000000000000, 1.000000000000000000, -4.880644499660747568E-12 ) ) ;
#8567 = CARTESIAN_POINT ( 'NONE',  ( 0.000000000000000000, 1.622047244094488638, 0.000000000000000000 ) ) ;
#8568 = ADVANCED_FACE ( 'NONE', ( #4012 ), #11217, .T. ) ;
#8569 = CARTESIAN_POINT ( 'NONE',  ( -1.417802900492933782, -0.04287136159519133044, 0.07874015748031495954 ) ) ;
#8570 = CARTESIAN_POINT ( 'NONE',  ( 1.976792077363838002E-17, -0.1023622047244094474, 0.1614173228346456879 ) ) ;
#8571 = ORIENTED_EDGE ( 'NONE', *, *, #4614, .T. ) ;
#8572 = ORIENTED_EDGE ( 'NONE', *, *, #2599, .T. ) ;
#8573 = TOROIDAL_SURFACE ( 'NONE', #13326, 0.5433070866141731514, 0.007874015748031495954 ) ;
#8574 = EDGE_LOOP ( 'NONE', ( #3830, #339, #13333 ) ) ;
#8575 = TOROIDAL_SURFACE ( 'NONE', #4081, 0.5984251968503937480, 0.007874015748031495954 ) ;
#8576 = AXIS2_PLACEMENT_3D ( 'NONE', #1066, #4746, #14377 ) ;
#8577 = FACE_OUTER_BOUND ( 'NONE', #15358, .T. ) ;
#8578 = FACE_OUTER_BOUND ( 'NONE', #11842, .T. ) ;
#8579 = EDGE_CURVE ( 'NONE', #14086, #4146, #9149, .T. ) ;
#8580 = CARTESIAN_POINT ( 'NONE',  ( -0.1028896637645180384, -0.4921259842519685179, -0.2462933508112025438 ) ) ;
#8581 = DIRECTION ( 'NONE',  ( -0.000000000000000000, -1.000000000000000000, -0.000000000000000000 ) ) ;
#8582 = FACE_OUTER_BOUND ( 'NONE', #4782, .T. ) ;
#8583 = CIRCLE ( 'NONE', #9586, 0.003937007874015724558 ) ;
#8584 = AXIS2_PLACEMENT_3D ( 'NONE', #7167, #3325, #15403 ) ;
#8585 = LINE ( 'NONE', #3810, #3150 ) ;
#8586 = EDGE_CURVE ( 'NONE', #9204, #7731, #3389, .T. ) ;
#8587 = CARTESIAN_POINT ( 'NONE',  ( -1.926743884294085829, -2.799928598775826671, -0.1541059977087025634 ) ) ;
#8588 = AXIS2_PLACEMENT_3D ( 'NONE', #6780, #6709, #836 ) ;
#8589 = ADVANCED_FACE ( 'NONE', ( #12829 ), #8393, .F. ) ;
#8590 = CARTESIAN_POINT ( 'NONE',  ( 0.06692913385832209572, -0.4921259842519685179, -0.2377126739437404879 ) ) ;
#8591 = CARTESIAN_POINT ( 'NONE',  ( 5.303588500244448531E-18, 8.003460918938271148E-19, -0.04330708661417326938 ) ) ;
#8592 = AXIS2_PLACEMENT_3D ( 'NONE', #5728, #9576, #10524 ) ;
#8593 = ORIENTED_EDGE ( 'NONE', *, *, #8189, .T. ) ;
#8594 = EDGE_LOOP ( 'NONE', ( #9427, #487 ) ) ;
#8595 = ORIENTED_EDGE ( 'NONE', *, *, #2904, .F. ) ;
#8596 = ORIENTED_EDGE ( 'NONE', *, *, #5371, .T. ) ;
#8597 = APPLICATION_CONTEXT ( 'automotive_design' ) ;
#8598 = ORIENTED_EDGE ( 'NONE', *, *, #276, .T. ) ;
#8599 = CIRCLE ( 'NONE', #3592, 0.003937007874015721089 ) ;
#8600 = AXIS2_PLACEMENT_3D ( 'NONE', #9684, #3724, #13270 ) ;
#8601 = DIRECTION ( 'NONE',  ( -1.000000000000000000, -0.000000000000000000, -3.973232667114495301E-16 ) ) ;
#8602 = CIRCLE ( 'NONE', #4345, 0.7007874015748031260 ) ;
#8603 = CIRCLE ( 'NONE', #8592, 0.003937007874015721089 ) ;
#8604 = DIRECTION ( 'NONE',  ( 0.8660254037844387076, 0.000000000000000000, 0.4999999999999996669 ) ) ;
#8605 = CARTESIAN_POINT ( 'NONE',  ( 0.5447670804913020692, 1.338597318737259734, 0.2463304438913534455 ) ) ;
#8606 = FACE_OUTER_BOUND ( 'NONE', #8255, .T. ) ;
#8607 = CARTESIAN_POINT ( 'NONE',  ( -2.176576600058865107, -2.015093358878988106, 0.09005837916847796165 ) ) ;
#8608 = DIRECTION ( 'NONE',  ( 1.000000000000000000, 0.000000000000000000, 0.000000000000000000 ) ) ;
#8609 = CARTESIAN_POINT ( 'NONE',  ( -1.906026250053923565, -2.926978850311991120, 0.08666856585884122333 ) ) ;
#8610 = ORIENTED_EDGE ( 'NONE', *, *, #13893, .F. ) ;
#8611 = CARTESIAN_POINT ( 'NONE',  ( -1.943752432982631007, -2.936018085428647062, -0.02335751294002252551 ) ) ;
#8612 = CARTESIAN_POINT ( 'NONE',  ( -1.584115185264708625, 0.1296286773226380806, 0.03937007874015747977 ) ) ;
#8613 = LINE ( 'NONE', #1497, #8712 ) ;
#8614 = ORIENTED_EDGE ( 'NONE', *, *, #8535, .T. ) ;
#8615 = AXIS2_PLACEMENT_3D ( 'NONE', #3599, #7271, #5854 ) ;
#8616 = ORIENTED_EDGE ( 'NONE', *, *, #6850, .F. ) ;
#8617 = CIRCLE ( 'NONE', #2849, 0.6692913385826770867 ) ;
#8618 = AXIS2_PLACEMENT_3D ( 'NONE', #6670, #5330, #10284 ) ;
#8619 = CARTESIAN_POINT ( 'NONE',  ( -1.431036756819011213, -0.02829858486107876200, -0.08366141732283460808 ) ) ;
#8620 = VERTEX_POINT ( 'NONE', #13554 ) ;
#8621 = CIRCLE ( 'NONE', #2856, 0.003937007874015742773 ) ;
#8622 = CIRCLE ( 'NONE', #1375, 0.1574803149606299191 ) ;
#8623 = CIRCLE ( 'NONE', #1876, 0.003937007874015724558 ) ;
#8624 = CLOSED_SHELL ( 'NONE', ( #608, #2546, #8969, #306, #847, #7315, #6301, #10278, #9788, #6152, #4149, #250, #14138, #12990, #2124, #10394 ) ) ;
#8625 = DIRECTION ( 'NONE',  ( -0.000000000000000000, 0.000000000000000000, 1.000000000000000000 ) ) ;
#8626 = DIRECTION ( 'NONE',  ( -0.000000000000000000, -0.000000000000000000, -1.000000000000000000 ) ) ;
#8627 = ITEM_DEFINED_TRANSFORMATION ( 'NONE', 'NONE', #10628,  #11481 ) ;
#8628 = VECTOR ( 'NONE', #7041, 39.37007874015748143 ) ;
#8629 = CARTESIAN_POINT ( 'NONE',  ( -0.04497577134311978031, -0.1837750859334940368, -0.03094209595079721806 ) ) ;
#8630 = ORIENTED_EDGE ( 'NONE', *, *, #11980, .F. ) ;
#8631 = EDGE_CURVE ( 'NONE', #11432, #9431, #13896, .T. ) ;
#8632 = FACE_BOUND ( 'NONE', #5789, .T. ) ;
#8633 = DIRECTION ( 'NONE',  ( 0.000000000000000000, -0.000000000000000000, 1.000000000000000000 ) ) ;
#8634 = CARTESIAN_POINT ( 'NONE',  ( -1.182292271279389295, 0.3416831649379189484, -0.04963307157686430715 ) ) ;
#8635 = CARTESIAN_POINT ( 'NONE',  ( -0.008240795940610745954, -0.1611877539686307204, 0.01644599795625022523 ) ) ;
#8636 = EDGE_CURVE ( 'NONE', #5052, #7977, #2389, .T. ) ;
#8637 = AXIS2_PLACEMENT_3D ( 'NONE', #13644, #13729, #12476 ) ;
#8638 = AXIS2_PLACEMENT_3D ( 'NONE', #7526, #13941, #332 ) ;
#8639 = AXIS2_PLACEMENT_3D ( 'NONE', #11827, #535, #2792 ) ;
#8640 = EDGE_LOOP ( 'NONE', ( #3535, #10292, #531, #794 ) ) ;
#8641 = EDGE_CURVE ( 'NONE', #7421, #748, #10897, .T. ) ;
#8642 = ORIENTED_EDGE ( 'NONE', *, *, #3698, .T. ) ;
#8643 = VERTEX_POINT ( 'NONE', #2100 ) ;
#8644 = AXIS2_PLACEMENT_3D ( 'NONE', #6543, #14964, #620 ) ;
#8645 = ORIENTED_EDGE ( 'NONE', *, *, #2241, .T. ) ;
#8646 = DIRECTION ( 'NONE',  ( 0.8660254037844385966, 0.000000000000000000, -0.5000000000000000000 ) ) ;
#8647 = LINE ( 'NONE', #7934, #12908 ) ;
#8648 = DIRECTION ( 'NONE',  ( 0.000000000000000000, 0.000000000000000000, 1.000000000000000000 ) ) ;
#8649 = CARTESIAN_POINT ( 'NONE',  ( -0.3441669734936866343, 2.010494531933507467, -0.03937007874015747977 ) ) ;
#8650 = DIRECTION ( 'NONE',  ( 5.551115123125782702E-17, 0.5004167495348750272, 0.8657846595920662969 ) ) ;
#8651 = AXIS2_PLACEMENT_3D ( 'NONE', #503, #11292, #14595 ) ;
#8652 = CARTESIAN_POINT ( 'NONE',  ( -0.4803149606299220720, -0.4921259842519685179, 0.3500470136031578194 ) ) ;
#8653 = AXIS2_PLACEMENT_3D ( 'NONE', #3813, #9941, #6383 ) ;
#8654 = LINE ( 'NONE', #15261, #15375 ) ;
#8655 = AXIS2_PLACEMENT_3D ( 'NONE', #341, #2529, #2468 ) ;
#8656 = ADVANCED_FACE ( 'NONE', ( #5533 ), #6619, .T. ) ;
#8657 = DIRECTION ( 'NONE',  ( 0.000000000000000000, 0.000000000000000000, -1.000000000000000000 ) ) ;
#8658 = DIRECTION ( 'NONE',  ( -0.000000000000000000, -1.000000000000000000, -0.000000000000000000 ) ) ;
#8659 = CARTESIAN_POINT ( 'NONE',  ( -1.580080891953811628, 0.1020406297922293037, -0.08366141732283462196 ) ) ;
#8660 = EDGE_CURVE ( 'NONE', #8071, #9541, #11136, .T. ) ;
#8661 = PLANE ( 'NONE',  #1668 ) ;
#8662 = ORIENTED_EDGE ( 'NONE', *, *, #6520, .T. ) ;
#8663 = EDGE_CURVE ( 'NONE', #5876, #4883, #4890, .T. ) ;
#8664 = ADVANCED_FACE ( 'NONE', ( #12764 ), #3935, .F. ) ;
#8665 = EDGE_LOOP ( 'NONE', ( #13248, #9032, #2524, #4495 ) ) ;
#8666 = AXIS2_PLACEMENT_3D ( 'NONE', #4971, #9769, #13352 ) ;
#8667 = VERTEX_POINT ( 'NONE', #14015 ) ;
#8668 = AXIS2_PLACEMENT_3D ( 'NONE', #6443, #5426, #13568 ) ;
#8669 = CARTESIAN_POINT ( 'NONE',  ( 0.3635801767928728556, -0.2952755905511811330, 0.2871962198427739921 ) ) ;
#8670 = CARTESIAN_POINT ( 'NONE',  ( -1.941063491063433677, -2.942568514135356583, 0.04947710996518819848 ) ) ;
#8671 = DIRECTION ( 'NONE',  ( -0.000000000000000000, -1.000000000000000000, -0.000000000000000000 ) ) ;
#8672 = DIRECTION ( 'NONE',  ( 0.000000000000000000, -0.000000000000000000, 1.000000000000000000 ) ) ;
#8673 = CARTESIAN_POINT ( 'NONE',  ( 0.000000000000000000, 0.000000000000000000, 0.000000000000000000 ) ) ;
#8674 = CARTESIAN_POINT ( 'NONE',  ( 8.678599364036360127E-17, 1.385826771653543510, 0.7086614173228346081 ) ) ;
#8675 = VECTOR ( 'NONE', #1284, 39.37007874015748143 ) ;
#8676 = DIRECTION ( 'NONE',  ( 0.000000000000000000, 0.000000000000000000, -1.000000000000000000 ) ) ;
#8677 = CARTESIAN_POINT ( 'NONE',  ( -1.895365998581063360, -2.883386225592859287, 0.1045859054727397014 ) ) ;
#8678 = CARTESIAN_POINT ( 'NONE',  ( -0.1724006475077544398, -0.4881889763779528324, 0.1768186671464649640 ) ) ;
#8679 = DIRECTION ( 'NONE',  ( 0.000000000000000000, 1.000000000000000000, 0.000000000000000000 ) ) ;
#8680 = CIRCLE ( 'NONE', #6919, 0.03937007874015752140 ) ;
#8681 = ORIENTED_EDGE ( 'NONE', *, *, #4986, .F. ) ;
#8682 = EDGE_CURVE ( 'NONE', #13131, #13558, #15407, .T. ) ;
#8683 = VERTEX_POINT ( 'NONE', #3277 ) ;
#8684 = EDGE_CURVE ( 'NONE', #4631, #9513, #6788, .T. ) ;
#8685 = ORIENTED_EDGE ( 'NONE', *, *, #9165, .T. ) ;
#8686 = ORIENTED_EDGE ( 'NONE', *, *, #6520, .F. ) ;
#8687 = ORIENTED_EDGE ( 'NONE', *, *, #5257, .T. ) ;
#8688 = AXIS2_PLACEMENT_3D ( 'NONE', #12597, #13776, #3040 ) ;
#8689 = DIRECTION ( 'NONE',  ( -0.000000000000000000, -1.000000000000000000, -0.000000000000000000 ) ) ;
#8690 = EDGE_CURVE ( 'NONE', #13179, #11605, #8718, .T. ) ;
#8691 = DIRECTION ( 'NONE',  ( -0.8660254037844341557, -0.000000000000000000, -0.5000000000000079936 ) ) ;
#8692 = CIRCLE ( 'NONE', #1683, 0.01968503937007872948 ) ;
#8693 = PRODUCT ( 'Bolt', 'Bolt', '', ( #12493 ) ) ;
#8694 = DIRECTION ( 'NONE',  ( -0.000000000000000000, 1.000000000000000000, 0.000000000000000000 ) ) ;
#8695 = CARTESIAN_POINT ( 'NONE',  ( -1.964126537190518107, -2.752050336136263819, 0.1561691687464110412 ) ) ;
#8696 = VECTOR ( 'NONE', #12017, 39.37007874015748143 ) ;
#8697 = CARTESIAN_POINT ( 'NONE',  ( -2.119211488178836866, -2.391206066311296841, 0.1145569965097087001 ) ) ;
#8698 = CARTESIAN_POINT ( 'NONE',  ( -0.1771653543307086243, -0.02638708502139245488, -0.05905511811023622659 ) ) ;
#8699 = CARTESIAN_POINT ( 'NONE',  ( -1.871152938270946642, -2.943146576430611727, -0.04758650140680115159 ) ) ;
#8700 = ORIENTED_EDGE ( 'NONE', *, *, #2530, .F. ) ;
#8701 = CARTESIAN_POINT ( 'NONE',  ( -2.099929645848620297, -2.385360057865189454, -0.1341722008959704004 ) ) ;
#8702 = AXIS2_PLACEMENT_3D ( 'NONE', #459, #1277, #2002 ) ;
#8703 = EDGE_LOOP ( 'NONE', ( #3545, #13267 ) ) ;
#8704 = ORIENTED_EDGE ( 'NONE', *, *, #77, .T. ) ;
#8705 = VECTOR ( 'NONE', #13733, 39.37007874015748143 ) ;
#8706 = ORIENTED_EDGE ( 'NONE', *, *, #12026, .T. ) ;
#8707 = EDGE_CURVE ( 'NONE', #13646, #2728, #6373, .T. ) ;
#8708 = CIRCLE ( 'NONE', #14233, 0.007874015748031516770 ) ;
#8709 = CARTESIAN_POINT ( 'NONE',  ( -2.184126211765464287, -1.725292181286280480, 0.1968503937007874127 ) ) ;
#8710 = CARTESIAN_POINT ( 'NONE',  ( 0.4769054117961250561, -0.1023622047244094474, 0.3480785096661500599 ) ) ;
#8711 = CARTESIAN_POINT ( 'NONE',  ( 0.5412478373021326616, 1.346456692913385877, 0.2362233606508025163 ) ) ;
#8712 = VECTOR ( 'NONE', #7216, 39.37007874015748143 ) ;
#8713 = CARTESIAN_POINT ( 'NONE',  ( -0.05114323250695503725, 0.05905511811023622659, -0.08858267716535432601 ) ) ;
#8714 = CARTESIAN_POINT ( 'NONE',  ( -0.04489327544264908737, -0.1650454269528150719, -0.05194604157257243227 ) ) ;
#8715 = VERTEX_POINT ( 'NONE', #15106 ) ;
#8716 = DIRECTION ( 'NONE',  ( -0.000000000000000000, -1.000000000000000000, -0.000000000000000000 ) ) ;
#8717 = CARTESIAN_POINT ( 'NONE',  ( -0.08413922508867374694, 0.06963377358823465146, 0.006254882657694874927 ) ) ;
#8718 = LINE ( 'NONE', #8786, #14149 ) ;
#8719 = DIRECTION ( 'NONE',  ( 0.000000000000000000, 0.000000000000000000, -1.000000000000000000 ) ) ;
#8720 = DIRECTION ( 'NONE',  ( 0.000000000000000000, 2.212657494868377674E-16, 1.000000000000000000 ) ) ;
#8721 = CIRCLE ( 'NONE', #2962, 0.003937007874015724558 ) ;
#8722 = VERTEX_POINT ( 'NONE', #8226 ) ;
#8723 = EDGE_LOOP ( 'NONE', ( #4958, #2024, #8103, #10105 ) ) ;
#8724 = ORIENTED_EDGE ( 'NONE', *, *, #9165, .F. ) ;
#8725 = DIRECTION ( 'NONE',  ( -1.000000000000000000, -1.734723475976817507E-14, 0.000000000000000000 ) ) ;
#8726 = DIRECTION ( 'NONE',  ( 1.000000000000000000, -0.000000000000000000, -0.000000000000000000 ) ) ;
#8727 = EDGE_CURVE ( 'NONE', #7319, #12058, #11671, .T. ) ;
#8728 = CARTESIAN_POINT ( 'NONE',  ( -0.08151194962748890827, 0.1637246173173402264, -0.03937007874015747977 ) ) ;
#8729 = DIRECTION ( 'NONE',  ( 0.000000000000000000, 0.000000000000000000, 1.000000000000000000 ) ) ;
#8730 = CARTESIAN_POINT ( 'NONE',  ( -1.408713103043102821, -0.006839756437906783539, 0.06104195403929376512 ) ) ;
#8731 = CARTESIAN_POINT ( 'NONE',  ( 0.000000000000000000, 0.3228346456692913757, 0.000000000000000000 ) ) ;
#8732 = DIRECTION ( 'NONE',  ( 0.000000000000000000, -0.000000000000000000, -1.000000000000000000 ) ) ;
#8733 = EDGE_CURVE ( 'NONE', #5753, #1627, #10398, .T. ) ;
#8734 = LINE ( 'NONE', #1757, #8346 ) ;
#8735 = DIRECTION ( 'NONE',  ( 0.000000000000000000, 0.000000000000000000, 1.000000000000000000 ) ) ;
#8736 = DIRECTION ( 'NONE',  ( -0.8660254037844388186, 0.000000000000000000, 0.4999999999999995559 ) ) ;
#8737 = EDGE_LOOP ( 'NONE', ( #6199, #8125, #4637, #11824, #6587 ) ) ;
#8738 = ORIENTED_EDGE ( 'NONE', *, *, #10367, .T. ) ;
#8739 = VERTEX_POINT ( 'NONE', #12921 ) ;
#8740 = EDGE_LOOP ( 'NONE', ( #2039, #2810, #6454, #2248 ) ) ;
#8741 = EDGE_CURVE ( 'NONE', #1544, #12965, #12651, .T. ) ;
#8742 = EDGE_CURVE ( 'NONE', #3832, #11872, #7034, .T. ) ;
#8743 = CARTESIAN_POINT ( 'NONE',  ( 0.2953892001169327042, -0.2952755905511811330, 0.2478261411026164707 ) ) ;
#8744 = CARTESIAN_POINT ( 'NONE',  ( -1.949387861892222018, -2.922373346087915547, 0.09505135847318786635 ) ) ;
#8745 = DIRECTION ( 'NONE',  ( -0.000000000000000000, 1.000000000000000000, 0.000000000000000000 ) ) ;
#8746 = LINE ( 'NONE', #11489, #1944 ) ;
#8747 = ADVANCED_FACE ( 'NONE', ( #9629 ), #8902, .T. ) ;
#8748 = PLANE ( 'NONE',  #2090 ) ;
#8749 = CARTESIAN_POINT ( 'NONE',  ( -1.452763252956529083, -0.05091287232363064796, -0.08366141732283456645 ) ) ;
#8750 = FACE_OUTER_BOUND ( 'NONE', #5678, .T. ) ;
#8751 = CARTESIAN_POINT ( 'NONE',  ( -1.881730119666213508, -2.917306682172244869, 0.03996051238533837591 ) ) ;
#8752 = CARTESIAN_POINT ( 'NONE',  ( -0.06692913385815728311, -0.2952755905511811330, -0.4190977005962941426 ) ) ;
#8753 = DIRECTION ( 'NONE',  ( -0.000000000000000000, -1.000000000000000000, -0.000000000000000000 ) ) ;
#8754 = ORIENTED_EDGE ( 'NONE', *, *, #5196, .T. ) ;
#8755 = ORIENTED_EDGE ( 'NONE', *, *, #2432, .T. ) ;
#8756 = VERTEX_POINT ( 'NONE', #14407 ) ;
#8757 = EDGE_LOOP ( 'NONE', ( #11957, #4511, #12590, #14412 ) ) ;
#8758 = ORIENTED_EDGE ( 'NONE', *, *, #14704, .T. ) ;
#8759 = EDGE_CURVE ( 'NONE', #8022, #6733, #7195, .T. ) ;
#8760 = CARTESIAN_POINT ( 'NONE',  ( -1.391815368240343576, -0.02267036402578939333, -0.03937007906611866836 ) ) ;
#8761 = CARTESIAN_POINT ( 'NONE',  ( 0.5615510810874363434, -0.09448818897637796532, 0.2014679098129276424 ) ) ;
#8762 = DIRECTION ( 'NONE',  ( 0.000000000000000000, 0.000000000000000000, 1.000000000000000000 ) ) ;
#8763 = EDGE_CURVE ( 'NONE', #1004, #12588, #13773, .T. ) ;
#8764 = CARTESIAN_POINT ( 'NONE',  ( -0.5445274672588088505, 1.043263280880422528, 0.2461921031270815630 ) ) ;
#8765 = EDGE_CURVE ( 'NONE', #4146, #9812, #9483, .T. ) ;
#8766 = CARTESIAN_POINT ( 'NONE',  ( 0.000000000000000000, 0.5590551181102362266, -0.5511811023622046335 ) ) ;
#8767 = CARTESIAN_POINT ( 'NONE',  ( -1.185322244938940894, 0.3350014259199165512, 0.05695314934226588383 ) ) ;
#8768 = CARTESIAN_POINT ( 'NONE',  ( -1.887765756933061478, -2.902443322690533734, 0.07703872521121671313 ) ) ;
#8769 = ORIENTED_EDGE ( 'NONE', *, *, #9977, .F. ) ;
#8770 = CARTESIAN_POINT ( 'NONE',  ( -0.1743691514447623103, -0.4921259842519685179, 0.1734091183126679758 ) ) ;
#8771 = B_SPLINE_CURVE_WITH_KNOTS ( 'NONE', 3,
 ( #1934, #758, #12348, #4346 ),
 .UNSPECIFIED., .F., .F.,
 ( 4, 4 ),
 ( 0.000000000000000000, 0.0001112824830758653706 ),
 .UNSPECIFIED. ) ;
#8772 = CARTESIAN_POINT ( 'NONE',  ( -1.572630165645712008, 0.1123721976951364415, 0.05999513677286145291 ) ) ;
#8773 = DIRECTION ( 'NONE',  ( -0.8660254037844385966, -0.000000000000000000, -0.5000000000000000000 ) ) ;
#8774 = EDGE_LOOP ( 'NONE', ( #12117, #8897 ) ) ;
#8775 = EDGE_CURVE ( 'NONE', #7883, #9377, #10558, .T. ) ;
#8776 = ORIENTED_EDGE ( 'NONE', *, *, #12488, .F. ) ;
#8777 = ORIENTED_EDGE ( 'NONE', *, *, #3035, .F. ) ;
#8778 = DIRECTION ( 'NONE',  ( 1.000000000000000000, 0.000000000000000000, 0.000000000000000000 ) ) ;
#8779 = DIRECTION ( 'NONE',  ( -0.8144815189573204606, 0.5801894994542525774, -1.283760644411384396E-16 ) ) ;
#8780 = EDGE_CURVE ( 'NONE', #11283, #9168, #5877, .T. ) ;
#8781 = DIRECTION ( 'NONE',  ( 0.000000000000000000, -0.000000000000000000, -1.000000000000000000 ) ) ;
#8782 = CARTESIAN_POINT ( 'NONE',  ( -0.002345674784311424250, -0.1605320876855827750, 0.0006089964461715403551 ) ) ;
#8783 = ORIENTED_EDGE ( 'NONE', *, *, #7114, .T. ) ;
#8784 = FACE_OUTER_BOUND ( 'NONE', #3658, .T. ) ;
#8785 = DIRECTION ( 'NONE',  ( 0.000000000000000000, 0.000000000000000000, -1.000000000000000000 ) ) ;
#8786 = CARTESIAN_POINT ( 'NONE',  ( 0.2652685895082805834, -0.1023622047244094474, 0.03495519865525829883 ) ) ;
#8787 = CARTESIAN_POINT ( 'NONE',  ( -0.01656597074380655038, -0.1797544903306448061, 0.02941166498823430051 ) ) ;
#8788 = EDGE_CURVE ( 'NONE', #11758, #11513, #6886, .T. ) ;
#8789 = FACE_OUTER_BOUND ( 'NONE', #321, .T. ) ;
#8790 = ORIENTED_EDGE ( 'NONE', *, *, #9137, .T. ) ;
#8791 = VERTEX_POINT ( 'NONE', #7106 ) ;
#8792 = ORIENTED_EDGE ( 'NONE', *, *, #14823, .T. ) ;
#8793 = CARTESIAN_POINT ( 'NONE',  ( -0.05114323250695500950, 0.05905511811023622659, 0.08858267716535433989 ) ) ;
#8794 = CARTESIAN_POINT ( 'NONE',  ( -1.417802900492933560, -0.04287136159519124717, -0.08366141732283458032 ) ) ;
#8795 = CARTESIAN_POINT ( 'NONE',  ( -2.042760673955246187, -2.379061152454923889, 0.1351464036074991604 ) ) ;
#8796 = FACE_OUTER_BOUND ( 'NONE', #5262, .T. ) ;
#8797 = DIRECTION ( 'NONE',  ( 1.000000000000000000, -8.673617379884049672E-15, -0.000000000000000000 ) ) ;
#8798 = FACE_OUTER_BOUND ( 'NONE', #10906, .T. ) ;
#8799 = CARTESIAN_POINT ( 'NONE',  ( -0.4121618538092056139, -0.2952755905511811330, 0.1243101294532692330 ) ) ;
#8800 = LINE ( 'NONE', #4968, #2325 ) ;
#8801 = CYLINDRICAL_SURFACE ( 'NONE', #9136, 0.003937007874015758385 ) ;
#8802 = CIRCLE ( 'NONE', #9807, 0.03937007874015761161 ) ;
#8803 = CARTESIAN_POINT ( 'NONE',  ( 0.000000000000000000, 0.3149606299212598381, 0.000000000000000000 ) ) ;
#8804 = ORIENTED_EDGE ( 'NONE', *, *, #13389, .T. ) ;
#8805 = EDGE_LOOP ( 'NONE', ( #11725, #8984, #15454, #8196 ) ) ;
#8806 = ORIENTED_EDGE ( 'NONE', *, *, #14299, .T. ) ;
#8807 = ORIENTED_EDGE ( 'NONE', *, *, #13355, .F. ) ;
#8808 = DIRECTION ( 'NONE',  ( -1.000000000000000000, 0.000000000000000000, 0.000000000000000000 ) ) ;
#8809 = CARTESIAN_POINT ( 'NONE',  ( -1.945324558181595664, -2.932205473225905301, -0.04017210842460155334 ) ) ;
#8810 = DIRECTION ( 'NONE',  ( 1.000000000000000000, -0.000000000000000000, -0.000000000000000000 ) ) ;
#8811 = CARTESIAN_POINT ( 'NONE',  ( 0.1804058482825207921, -0.4881889763779528324, -0.1041573650692961123 ) ) ;
#8812 = DIRECTION ( 'NONE',  ( 0.8660254037844390407, 0.000000000000000000, -0.4999999999999994449 ) ) ;
#8813 = DIRECTION ( 'NONE',  ( 0.8660254037844385966, 0.000000000000000000, 0.5000000000000000000 ) ) ;
#8814 = CARTESIAN_POINT ( 'NONE',  ( 0.07874015748031494566, 0.1699885096953269725, 0.03937007874015747977 ) ) ;
#8815 = CARTESIAN_POINT ( 'NONE',  ( -1.938093919480919469, -2.767579153824591742, -0.1578472193797151868 ) ) ;
#8816 = ADVANCED_FACE ( 'NONE', ( #4603 ), #15342, .T. ) ;
#8817 = DIRECTION ( 'NONE',  ( -1.301042606982607687E-14, 0.000000000000000000, 1.000000000000000000 ) ) ;
#8818 = DIRECTION ( 'NONE',  ( -0.8660254037844385966, 0.000000000000000000, -0.5000000000000000000 ) ) ;
#8819 = CIRCLE ( 'NONE', #6057, 0.003937007874015749712 ) ;
#8820 = EDGE_CURVE ( 'NONE', #14360, #6809, #5841, .T. ) ;
#8821 = ORIENTED_EDGE ( 'NONE', *, *, #13927, .T. ) ;
#8822 = ORIENTED_EDGE ( 'NONE', *, *, #4003, .F. ) ;
#8823 = VERTEX_POINT ( 'NONE', #10643 ) ;
#8824 = ORIENTED_EDGE ( 'NONE', *, *, #256, .T. ) ;
#8825 = ADVANCED_FACE ( 'NONE', ( #14253 ), #14654, .T. ) ;
#8826 = VERTEX_POINT ( 'NONE', #8289 ) ;
#8827 = CARTESIAN_POINT ( 'NONE',  ( -0.03346456692913319514, -0.4881889763779528324, 0.05796233017454789638 ) ) ;
#8828 = LINE ( 'NONE', #3770, #7832 ) ;
#8829 = DIRECTION ( 'NONE',  ( -0.000000000000000000, 1.000000000000000000, -0.000000000000000000 ) ) ;
#8830 = AXIS2_PLACEMENT_3D ( 'NONE', #8173, #11847, #9507 ) ;
#8831 = CIRCLE ( 'NONE', #333, 1.865354330708661745 ) ;
#8832 = CARTESIAN_POINT ( 'NONE',  ( -0.06299212598414161146, -0.4881889763779528324, -0.5909884645248154600 ) ) ;
#8833 = TOROIDAL_SURFACE ( 'NONE', #7320, 0.6614173228346456046, 0.007874015748031495954 ) ;
#8834 = DIRECTION ( 'NONE',  ( 0.000000000000000000, 0.000000000000000000, -1.000000000000000000 ) ) ;
#8835 = DIRECTION ( 'NONE',  ( 0.000000000000000000, 0.000000000000000000, -1.000000000000000000 ) ) ;
#8836 = AXIS2_PLACEMENT_3D ( 'NONE', #7811, #7741, #621 ) ;
#8837 = CARTESIAN_POINT ( 'NONE',  ( -0.1724006475077544398, -0.4921259842519685179, 0.1728816592724491952 ) ) ;
#8838 = LINE ( 'NONE', #10315, #12736 ) ;
#8839 = B_SPLINE_CURVE_WITH_KNOTS ( 'NONE', 3,
 ( #15018, #5132, #10002, #4117 ),
 .UNSPECIFIED., .F., .F.,
 ( 4, 4 ),
 ( 0.0001112824830758653706, 0.0003582764151311737771 ),
 .UNSPECIFIED. ) ;
#8840 = CARTESIAN_POINT ( 'NONE',  ( -1.899963887369776172, -2.943774530195527372, 0.04512397944535982697 ) ) ;
#8841 = ORIENTED_EDGE ( 'NONE', *, *, #10832, .F. ) ;
#8842 = CARTESIAN_POINT ( 'NONE',  ( -2.054794062201786176, -2.568933014739907872, -0.1522411129243764483 ) ) ;
#8843 = EDGE_CURVE ( 'NONE', #9186, #10277, #7887, .T. ) ;
#8844 = DIRECTION ( 'NONE',  ( -0.000000000000000000, -1.000000000000000000, -0.000000000000000000 ) ) ;
#8845 = CARTESIAN_POINT ( 'NONE',  ( -0.02952755905511744716, -0.09842519685039370636, 0.05114323250695388540 ) ) ;
#8846 = EDGE_CURVE ( 'NONE', #4047, #13856, #5368, .T. ) ;
#8847 = VERTEX_POINT ( 'NONE', #13147 ) ;
#8848 = EDGE_LOOP ( 'NONE', ( #7717, #8070, #9360, #264 ) ) ;
#8849 = AXIS2_PLACEMENT_3D ( 'NONE', #13581, #12508, #12272 ) ;
#8850 = AXIS2_PLACEMENT_3D ( 'NONE', #10158, #2861, #3975 ) ;
#8851 = AXIS2_PLACEMENT_3D ( 'NONE', #5952, #2209, #1034 ) ;
#8852 = EDGE_CURVE ( 'NONE', #2525, #851, #1251, .T. ) ;
#8853 = AXIS2_PLACEMENT_3D ( 'NONE', #11364, #2036, #8958 ) ;
#8854 = EDGE_CURVE ( 'NONE', #11475, #6409, #5890, .T. ) ;
#8855 = VERTEX_POINT ( 'NONE', #14787 ) ;
#8856 = DIRECTION ( 'NONE',  ( -0.000000000000000000, -1.000000000000000000, -0.000000000000000000 ) ) ;
#8857 = CARTESIAN_POINT ( 'NONE',  ( 7.135737254874341425E-17, 0.007874015748031480341, -0.5826771653543306728 ) ) ;
#8858 = VECTOR ( 'NONE', #14075, 39.37007874015748143 ) ;
#8859 = CARTESIAN_POINT ( 'NONE',  ( -0.4815353412745563833, 0.000000000000000000, 0.3552976658085854056 ) ) ;
#8860 = TOROIDAL_SURFACE ( 'NONE', #597, 0.5984251968503937480, 0.007874015748031495954 ) ;
#8861 = CARTESIAN_POINT ( 'NONE',  ( -0.6241293575972478580, -0.2952755905511811330, -0.3215685141414794113 ) ) ;
#8862 = ORIENTED_EDGE ( 'NONE', *, *, #7214, .T. ) ;
#8863 = CARTESIAN_POINT ( 'NONE',  ( -2.100501784635051550, -1.630597114118274238, 0.1033464566929129663 ) ) ;
#8864 = AXIS2_PLACEMENT_3D ( 'NONE', #8424, #11800, #12035 ) ;
#8865 = AXIS2_PLACEMENT_3D ( 'NONE', #8064, #9873, #3920 ) ;
#8866 = DIRECTION ( 'NONE',  ( -1.000000000000000000, 0.000000000000000000, 0.000000000000000000 ) ) ;
#8867 = AXIS2_PLACEMENT_3D ( 'NONE', #12642, #5495, #15062 ) ;
#8868 = CARTESIAN_POINT ( 'NONE',  ( 0.4751993499420013034, 0.000000000000000000, 0.3506226965216235336 ) ) ;
#8869 = CARTESIAN_POINT ( 'NONE',  ( -1.172017912842092668, 0.3609012623030120603, 0.05905511811023622659 ) ) ;
#8870 = AXIS2_PLACEMENT_3D ( 'NONE', #6354, #434, #5184 ) ;
#8871 = PRESENTATION_STYLE_ASSIGNMENT (( #5487 ) ) ;
#8872 = ORIENTED_EDGE ( 'NONE', *, *, #235, .T. ) ;
#8873 = EDGE_CURVE ( 'NONE', #2210, #1254, #6902, .T. ) ;
#8875 = ORIENTED_EDGE ( 'NONE', *, *, #6594, .F. ) ;
#8874 = AXIS2_PLACEMENT_3D ( 'NONE', #8974, #1820, #13747 ) ;
#8876 = AXIS2_PLACEMENT_3D ( 'NONE', #6395, #7806, #14733 ) ;
#8877 = VECTOR ( 'NONE', #13316, 39.37007874015748143 ) ;
#8878 = ORIENTED_EDGE ( 'NONE', *, *, #9246, .F. ) ;
#8879 = VECTOR ( 'NONE', #13233, 39.37007874015748143 ) ;
#8880 = DIRECTION ( 'NONE',  ( -1.504632769052536979E-28, 8.673617379884035472E-15, 1.000000000000000000 ) ) ;
#8881 = FACE_OUTER_BOUND ( 'NONE', #14189, .T. ) ;
#8882 = AXIS2_PLACEMENT_3D ( 'NONE', #8950, #7914, #3139 ) ;
#8883 = EDGE_CURVE ( 'NONE', #12332, #450, #1266, .T. ) ;
#8884 = CARTESIAN_POINT ( 'NONE',  ( -2.030417246223212402, -2.521630590619702961, 0.1490281301122292346 ) ) ;
#8885 = CARTESIAN_POINT ( 'NONE',  ( -0.1062992125983150127, -0.1023622047244094474, -0.2482618547482104143 ) ) ;
#8886 = DIRECTION ( 'NONE',  ( 0.5000000000000025535, -8.326672684688674053E-17, -0.8660254037844370423 ) ) ;
#8887 = DIRECTION ( 'NONE',  ( 0.000000000000000000, 0.000000000000000000, 1.000000000000000000 ) ) ;
#8888 = CARTESIAN_POINT ( 'NONE',  ( 0.04921259842516965272, -0.4921259842519685179, -0.08523872084487793543 ) ) ;
#8889 = DIRECTION ( 'NONE',  ( 0.5000000000000041078, -0.000000000000000000, 0.8660254037844363761 ) ) ;
#8890 = CARTESIAN_POINT ( 'NONE',  ( -0.06692913385815726923, -0.2952755905511811330, -0.4584677793364516640 ) ) ;
#8891 = DIRECTION ( 'NONE',  ( -0.5000000000000001110, 0.000000000000000000, 0.8660254037844388186 ) ) ;
#8892 = AXIS2_PLACEMENT_3D ( 'NONE', #5012, #13026, #7062 ) ;
#8893 = VECTOR ( 'NONE', #8977, 39.37007874015748143 ) ;
#8894 = AXIS2_PLACEMENT_3D ( 'NONE', #13038, #11421, #3417 ) ;
#8895 = CARTESIAN_POINT ( 'NONE',  ( 0.4857119623810668974, 1.338597318737259734, 0.3486169089052639780 ) ) ;
#8896 = AXIS2_PLACEMENT_3D ( 'NONE', #10406, #15262, #11503 ) ;
#8897 = ORIENTED_EDGE ( 'NONE', *, *, #11703, .T. ) ;
#8898 = DIRECTION ( 'NONE',  ( -0.000000000000000000, 1.000000000000000000, -0.000000000000000000 ) ) ;
#8899 = ORIENTED_EDGE ( 'NONE', *, *, #1959, .F. ) ;
#8900 = ORIENTED_EDGE ( 'NONE', *, *, #11027, .F. ) ;
#8901 = TOROIDAL_SURFACE ( 'NONE', #13652, 0.2165354330708662012, 0.01968503937007873988 ) ;
#8902 = TOROIDAL_SURFACE ( 'NONE', #8148, 0.1535433070866141780, 0.003937007874015747977 ) ;
#8903 = CIRCLE ( 'NONE', #2148, 0.04330708661417330407 ) ;
#8904 = SHAPE_REPRESENTATION ( 'MAT-022', ( #2610, #5205, #3865, #7602, #14877, #373, #859, #10863, #9626, #619, #3365, #5347, #6600, #10125, #11370, #1866, #8121, #10628, #12130, #14127, #4110, #7357, #4363, #2366, #6351, #2853, #9882, #3120, #8870, #6096 ), #9378 ) ;
#8905 = CARTESIAN_POINT ( 'NONE',  ( 0.6864776960422569463, 1.043307086614173151, 0.4645290592786023298 ) ) ;
#8906 = CARTESIAN_POINT ( 'NONE',  ( -1.945459748359985142, -2.745801194614594820, -0.1561691687464109024 ) ) ;
#8907 = CIRCLE ( 'NONE', #400, 0.003937007874015758385 ) ;
#8908 = CARTESIAN_POINT ( 'NONE',  ( -0.5610236220472173407, -0.1023622047244094474, 0.2102555114175287954 ) ) ;
#8909 = CARTESIAN_POINT ( 'NONE',  ( -1.988219667330677565, -2.822309060621705168, -0.1701858252292633988 ) ) ;
#8910 = DIRECTION ( 'NONE',  ( -0.000000000000000000, -1.000000000000000000, -0.000000000000000000 ) ) ;
#8911 = CARTESIAN_POINT ( 'NONE',  ( 8.196454954923229282E-17, 0.000000000000000000, 0.6692913385826770867 ) ) ;
#8912 = CARTESIAN_POINT ( 'NONE',  ( -1.898314360964700853, -2.875886787523748822, -0.1125291835257540562 ) ) ;
#8913 = CARTESIAN_POINT ( 'NONE',  ( 0.000000000000000000, 1.425196850393700920, 0.000000000000000000 ) ) ;
#8914 = CARTESIAN_POINT ( 'NONE',  ( -1.964126537190516331, -2.749515453455443570, -0.1756903148397133685 ) ) ;
#8915 = TOROIDAL_SURFACE ( 'NONE', #10163, 0.1535433070866141780, 0.003937007874015747977 ) ;
#8916 = CIRCLE ( 'NONE', #8410, 0.2106299212598415904 ) ;
#8917 = AXIS2_PLACEMENT_3D ( 'NONE', #537, #11329, #14874 ) ;
#8918 = VERTEX_POINT ( 'NONE', #8591 ) ;
#8919 = ORIENTED_EDGE ( 'NONE', *, *, #14101, .T. ) ;
#8920 = ORIENTED_EDGE ( 'NONE', *, *, #10654, .F. ) ;
#8921 = AXIS2_PLACEMENT_3D ( 'NONE', #10449, #10523, #11621 ) ;
#8922 = EDGE_LOOP ( 'NONE', ( #11181, #10631, #13628, #10037 ) ) ;
#8923 = EDGE_LOOP ( 'NONE', ( #8878, #14619, #5844, #610 ) ) ;
#8924 = CARTESIAN_POINT ( 'NONE',  ( -1.417127096045877499, -0.01082856000845578912, -0.06859240798594633259 ) ) ;
#8925 = EDGE_CURVE ( 'NONE', #10393, #2999, #1164, .T. ) ;
#8926 = B_SPLINE_CURVE_WITH_KNOTS ( 'NONE', 3,
 ( #3168, #7945, #8634, #108, #3782, #12172 ),
 .UNSPECIFIED., .F., .F.,
 ( 4, 2, 4 ),
 ( 4.336808689942017736E-19, 0.0003906509022999027445, 0.0007813018045998050554 ),
 .UNSPECIFIED. ) ;
#8927 = CARTESIAN_POINT ( 'NONE',  ( 7.232166136696967594E-17, 0.007874015748031480341, 0.5905511811023621549 ) ) ;
#8928 = FACE_OUTER_BOUND ( 'NONE', #9331, .T. ) ;
#8929 = VECTOR ( 'NONE', #13816, 39.37007874015748143 ) ;
#8930 = EDGE_CURVE ( 'NONE', #5518, #10807, #6633, .T. ) ;
#8931 = DIRECTION ( 'NONE',  ( -1.734723475976802677E-14, 0.000000000000000000, -1.000000000000000000 ) ) ;
#8932 = CARTESIAN_POINT ( 'NONE',  ( 0.4815353412745266848, 1.340095897400991554, 0.3474236500605469291 ) ) ;
#8933 = DIRECTION ( 'NONE',  ( 0.000000000000000000, 0.000000000000000000, 1.000000000000000000 ) ) ;
#8934 = DIRECTION ( 'NONE',  ( 0.000000000000000000, 0.000000000000000000, -1.000000000000000000 ) ) ;
#8935 = AXIS2_PLACEMENT_3D ( 'NONE', #4541, #14100, #10503 ) ;
#8936 = CARTESIAN_POINT ( 'NONE',  ( -1.869327508327784271, -2.947498318410580964, -0.02746507530585597448 ) ) ;
#8937 = ORIENTED_EDGE ( 'NONE', *, *, #6166, .T. ) ;
#8938 = CARTESIAN_POINT ( 'NONE',  ( -0.4121618538092055584, -0.2952755905511811330, 0.1243101294532693024 ) ) ;
#8939 = EDGE_CURVE ( 'NONE', #11243, #5281, #8165, .T. ) ;
#8940 = CARTESIAN_POINT ( 'NONE',  ( -0.5447670804912987386, 1.338597318737259734, 0.2463304438913610506 ) ) ;
#8941 = ORIENTED_EDGE ( 'NONE', *, *, #13596, .T. ) ;
#8942 = EDGE_LOOP ( 'NONE', ( #8999, #2271, #385, #1466 ) ) ;
#8943 = AXIS2_PLACEMENT_3D ( 'NONE', #13031, #2293, #7068 ) ;
#8944 = ORIENTED_EDGE ( 'NONE', *, *, #5272, .F. ) ;
#8945 = VECTOR ( 'NONE', #316, 39.37007874015748143 ) ;
#8946 = ADVANCED_FACE ( 'NONE', ( #11018 ), #5139, .F. ) ;
#8947 = AXIS2_PLACEMENT_3D ( 'NONE', #10285, #4315, #9113 ) ;
#8948 = EDGE_CURVE ( 'NONE', #12754, #3165, #9914, .T. ) ;
#8949 = CARTESIAN_POINT ( 'NONE',  ( -1.580080891953811628, 0.1020406297922293454, 0.07874015748031495954 ) ) ;
#8950 = CARTESIAN_POINT ( 'NONE',  ( 0.4339188594849086034, -0.2952755905511811330, 0.1732400634307316167 ) ) ;
#8951 = DIRECTION ( 'NONE',  ( 0.000000000000000000, 1.000000000000000000, 0.000000000000000000 ) ) ;
#8953 = VECTOR ( 'NONE', #6397, 39.37007874015748143 ) ;
#8952 = PLANE ( 'NONE',  #719 ) ;
#8954 = CARTESIAN_POINT ( 'NONE',  ( -1.452763252956527751, -0.05091287232363168880, 0.08366141732283458032 ) ) ;
#8955 = ORIENTED_EDGE ( 'NONE', *, *, #14036, .F. ) ;
#8956 = CARTESIAN_POINT ( 'NONE',  ( 0.3964138223131414840, -0.2952755905511811330, 0.1515865201236449578 ) ) ;
#8957 = ADVANCED_FACE ( 'NONE', ( #13458 ), #2725, .F. ) ;
#8958 = DIRECTION ( 'NONE',  ( -1.000000000000000000, 4.625929269271485914E-16, 0.000000000000000000 ) ) ;
#8959 = AXIS2_PLACEMENT_3D ( 'NONE', #14585, #3851, #7458 ) ;
#8960 = CARTESIAN_POINT ( 'NONE',  ( -0.01755170026722350021, -0.1621998028774611911, 0.03064271692327978289 ) ) ;
#8961 = DIRECTION ( 'NONE',  ( 0.8660254037844390407, 0.000000000000000000, -0.4999999999999995004 ) ) ;
#8962 = ORIENTED_EDGE ( 'NONE', *, *, #3769, .F. ) ;
#8963 = ORIENTED_EDGE ( 'NONE', *, *, #1999, .F. ) ;
#8964 = VECTOR ( 'NONE', #4198, 39.37007874015748143 ) ;
#8965 = ORIENTED_EDGE ( 'NONE', *, *, #6134, .T. ) ;
#8966 = CARTESIAN_POINT ( 'NONE',  ( 0.5445274672588121812, 1.190944881889763884, 0.2461921031270739857 ) ) ;
#8967 = CARTESIAN_POINT ( 'NONE',  ( -2.090051324975654268, -1.858423098537180129, 0.08664193191037310171 ) ) ;
#8968 = AXIS2_PLACEMENT_3D ( 'NONE', #3229, #8159, #5712 ) ;
#8969 = ADVANCED_FACE ( 'NONE', ( #7493 ), #1903, .T. ) ;
#8970 = CARTESIAN_POINT ( 'NONE',  ( -2.092336816894301954, -2.008044473685774545, 0.1095437400971965014 ) ) ;
#8971 = FACE_OUTER_BOUND ( 'NONE', #3087, .T. ) ;
#8972 = APPLICATION_PROTOCOL_DEFINITION ( 'draft international standard', 'automotive_design', 1998, #9207 ) ;
#8973 = DIRECTION ( 'NONE',  ( 0.000000000000000000, 0.000000000000000000, 1.000000000000000000 ) ) ;
#8974 = CARTESIAN_POINT ( 'NONE',  ( -0.09842519685028335019, -0.2952755905511811330, -0.4190977005962941981 ) ) ;
#8975 = CARTESIAN_POINT ( 'NONE',  ( -0.1022864650139100884, 0.05905511811023622659, -1.048351444896847144E-20 ) ) ;
#8976 = EDGE_CURVE ( 'NONE', #13096, #7977, #12916, .T. ) ;
#8977 = DIRECTION ( 'NONE',  ( 1.000000000000000000, -0.000000000000000000, -0.000000000000000000 ) ) ;
#8978 = CIRCLE ( 'NONE', #6703, 0.5905511811023621549 ) ;
#8979 = CARTESIAN_POINT ( 'NONE',  ( 0.4751993499420012479, 1.035433070866141891, 0.3506226965216235336 ) ) ;
#8980 = CIRCLE ( 'NONE', #5455, 0.04330708661417324162 ) ;
#8981 = ORIENTED_EDGE ( 'NONE', *, *, #14043, .T. ) ;
#8982 = EDGE_CURVE ( 'NONE', #13984, #4499, #2784, .T. ) ;
#8983 = ORIENTED_EDGE ( 'NONE', *, *, #8733, .T. ) ;
#8984 = ORIENTED_EDGE ( 'NONE', *, *, #10746, .T. ) ;
#8985 = CARTESIAN_POINT ( 'NONE',  ( 0.1181102362204724254, 2.440944881889764329, -0.03937007874015747977 ) ) ;
#8986 = CARTESIAN_POINT ( 'NONE',  ( -1.977060708627759400, -2.798357293484028396, 0.1753504056559904711 ) ) ;
#8987 = DIRECTION ( 'NONE',  ( 0.000000000000000000, 0.000000000000000000, 1.000000000000000000 ) ) ;
#8988 = CARTESIAN_POINT ( 'NONE',  ( -1.961618730074871753, -2.845436301845790439, -0.1618467189898775138 ) ) ;
#8989 = CARTESIAN_POINT ( 'NONE',  ( -0.1724006475077544953, -0.4881889763779528324, 0.1768186671464649640 ) ) ;
#8990 = CARTESIAN_POINT ( 'NONE',  ( -0.3441669734936866343, 2.010494531933507467, 0.03937007874015747977 ) ) ;
#8991 = DIRECTION ( 'NONE',  ( 0.8144815189573204606, -0.5801894994542525774, -1.283760644411384396E-16 ) ) ;
#8992 = FACE_OUTER_BOUND ( 'NONE', #14526, .T. ) ;
#8993 = ORIENTED_EDGE ( 'NONE', *, *, #3290, .T. ) ;
#8994 = EDGE_CURVE ( 'NONE', #14646, #10393, #8916, .T. ) ;
#8995 = EDGE_LOOP ( 'NONE', ( #1545, #7842, #3445 ) ) ;
#8996 = ORIENTED_EDGE ( 'NONE', *, *, #8660, .T. ) ;
#8997 = VERTEX_POINT ( 'NONE', #13593 ) ;
#8998 =( BOUNDED_CURVE ( )  B_SPLINE_CURVE ( 3, ( #14348, #5722, #8176, #5650 ),
 .UNSPECIFIED., .F., .T. ) 
 B_SPLINE_CURVE_WITH_KNOTS ( ( 4, 4 ),
 ( 0.000000000000000000, 1.570796326794894560 ),
 .UNSPECIFIED. ) 
 CURVE ( )  GEOMETRIC_REPRESENTATION_ITEM ( )  RATIONAL_B_SPLINE_CURVE ( ( 1.000000000000000000, 0.8047378541243654926, 0.8047378541243654926, 1.000000000000000000 ) ) 
 REPRESENTATION_ITEM ( '' )  );
#8999 = ORIENTED_EDGE ( 'NONE', *, *, #171, .F. ) ;
#9000 = CARTESIAN_POINT ( 'NONE',  ( -2.090051324975654268, -1.783311776966560736, 0.08466247786334288317 ) ) ;
#9001 = LINE ( 'NONE', #13774, #5312 ) ;
#9002 = DIRECTION ( 'NONE',  ( 0.000000000000000000, 0.000000000000000000, -1.000000000000000000 ) ) ;
#9003 = DIRECTION ( 'NONE',  ( -1.000000000000000000, 4.565061778886334044E-16, 0.000000000000000000 ) ) ;
#9004 = DIRECTION ( 'NONE',  ( 0.000000000000000000, 1.000000000000000000, 0.000000000000000000 ) ) ;
#9005 = CARTESIAN_POINT ( 'NONE',  ( 0.000000000000000000, 1.645669291338583085, 0.000000000000000000 ) ) ;
#9006 = CARTESIAN_POINT ( 'NONE',  ( 8.630384923125046426E-17, 1.653543307086614567, 0.7007874015748031260 ) ) ;
#9007 = DIRECTION ( 'NONE',  ( 1.445602896647339903E-16, 0.000000000000000000, -1.000000000000000000 ) ) ;
#9008 = CARTESIAN_POINT ( 'NONE',  ( -1.181342415303537230, 0.3435647566330583547, 0.04453711288980924388 ) ) ;
#9009 = CARTESIAN_POINT ( 'NONE',  ( -1.945364619566915643, -2.810512954809210928, -0.1731107110282803507 ) ) ;
#9010 = VERTEX_POINT ( 'NONE', #10008 ) ;
#9011 = DIRECTION ( 'NONE',  ( 1.000000000000000000, 0.000000000000000000, 0.000000000000000000 ) ) ;
#9012 = CARTESIAN_POINT ( 'NONE',  ( -1.584115185264708403, 0.1296286773226380251, 0.03937007874015747977 ) ) ;
#9013 = EDGE_LOOP ( 'NONE', ( #3801, #1691, #5120, #9680 ) ) ;
#9014 = ORIENTED_EDGE ( 'NONE', *, *, #14489, .T. ) ;
#9015 = ORIENTED_EDGE ( 'NONE', *, *, #6530, .F. ) ;
#9016 = EDGE_CURVE ( 'NONE', #11032, #5098, #10653, .T. ) ;
#9017 = FACE_OUTER_BOUND ( 'NONE', #12787, .T. ) ;
#9018 = CARTESIAN_POINT ( 'NONE',  ( 0.5860051159906326523, -0.09448818897637796532, 0.1591122789105293422 ) ) ;
#9019 = DIRECTION ( 'NONE',  ( -0.8660254037844397068, -0.000000000000000000, -0.4999999999999980571 ) ) ;
#9020 = DIRECTION ( 'NONE',  ( 0.000000000000000000, 1.000000000000000000, 0.000000000000000000 ) ) ;
#9021 = DIRECTION ( 'NONE',  ( 0.5801894994542512451, 0.8144815189573213488, -2.341876692568692102E-14 ) ) ;
#9022 = EDGE_LOOP ( 'NONE', ( #3815, #5842, #656, #10275 ) ) ;
#9023 = CARTESIAN_POINT ( 'NONE',  ( 0.000000000000000000, 1.614173228346457156, 0.000000000000000000 ) ) ;
#9024 = CARTESIAN_POINT ( 'NONE',  ( -0.4854723491485721798, 1.338626482899105241, 0.3484785681409913738 ) ) ;
#9025 = CARTESIAN_POINT ( 'NONE',  ( -1.419615703680148000, -0.01226548409420233354, -0.08366141732283458032 ) ) ;
#9026 = DIRECTION ( 'NONE',  ( -1.000000000000000000, 1.224646799147361096E-16, 0.000000000000000000 ) ) ;
#9027 = ORIENTED_EDGE ( 'NONE', *, *, #12522, .F. ) ;
#9028 = EDGE_CURVE ( 'NONE', #14809, #3677, #6069, .T. ) ;
#9029 = EDGE_CURVE ( 'NONE', #856, #14427, #1041, .T. ) ;
#9030 = ORIENTED_EDGE ( 'NONE', *, *, #10765, .T. ) ;
#9031 = ORIENTED_EDGE ( 'NONE', *, *, #9797, .F. ) ;
#9032 = ORIENTED_EDGE ( 'NONE', *, *, #8682, .T. ) ;
#9033 = EDGE_CURVE ( 'NONE', #2747, #15395, #12056, .T. ) ;
#9034 = CARTESIAN_POINT ( 'NONE',  ( 0.05905511811023622659, 1.190944881889763884, -0.7874015748031497619 ) ) ;
#9035 = FACE_OUTER_BOUND ( 'NONE', #10562, .T. ) ;
#9036 = DIRECTION ( 'NONE',  ( 0.000000000000000000, 0.000000000000000000, -1.000000000000000000 ) ) ;
#9037 = DIRECTION ( 'NONE',  ( 0.000000000000000000, -0.000000000000000000, 1.000000000000000000 ) ) ;
#9038 = PRODUCT_CONTEXT ( 'NONE', #8597, 'mechanical' ) ;
#9039 = DIRECTION ( 'NONE',  ( -1.000000000000000000, 0.000000000000000000, 0.000000000000000000 ) ) ;
#9040 = VERTEX_POINT ( 'NONE', #8517 ) ;
#9041 = CARTESIAN_POINT ( 'NONE',  ( -0.06299212598414161146, -0.1023622047244094474, -0.5870514566507987197 ) ) ;
#9042 = DIRECTION ( 'NONE',  ( 0.000000000000000000, 1.000000000000000000, 0.000000000000000000 ) ) ;
#9043 = DIRECTION ( 'NONE',  ( 0.000000000000000000, 0.000000000000000000, -1.000000000000000000 ) ) ;
#9044 = B_SPLINE_CURVE_WITH_KNOTS ( 'NONE', 3,
 ( #2361, #4725, #7146, #4557 ),
 .UNSPECIFIED., .F., .F.,
 ( 4, 4 ),
 ( 0.000000000000000000, 2.119993237936590205E-05 ),
 .UNSPECIFIED. ) ;
#9045 = ADVANCED_FACE ( 'NONE', ( #8992 ), #824, .F. ) ;
#9046 = DIRECTION ( 'NONE',  ( -1.000000000000000000, 0.000000000000000000, 0.000000000000000000 ) ) ;
#9047 = EDGE_CURVE ( 'NONE', #14387, #15025, #5449, .T. ) ;
#9048 = ORIENTED_EDGE ( 'NONE', *, *, #352, .F. ) ;
#9049 = ORIENTED_EDGE ( 'NONE', *, *, #8272, .T. ) ;
#9050 = ORIENTED_EDGE ( 'NONE', *, *, #12567, .T. ) ;
#9051 = ADVANCED_FACE ( 'NONE', ( #2958 ), #2867, .T. ) ;
#9052 = DIRECTION ( 'NONE',  ( -0.5801894994542512451, -0.8144815189573213488, 0.000000000000000000 ) ) ;
#9053 = CARTESIAN_POINT ( 'NONE',  ( -1.992382107315058049, -2.749515453455440905, 0.1756903148397118974 ) ) ;
#9054 = CARTESIAN_POINT ( 'NONE',  ( 7.328595018519593763E-17, 0.5984251968503937480, 0.5984251968503937480 ) ) ;
#9055 = CARTESIAN_POINT ( 'NONE',  ( -1.959346498473351739, -2.897603755323506558, -0.1049048269901905472 ) ) ;
#9056 = CARTESIAN_POINT ( 'NONE',  ( 0.000000000000000000, 5.629100846319917971E-17, -0.1614173228346456879 ) ) ;
#9057 = CARTESIAN_POINT ( 'NONE',  ( -0.05175539059627463218, 0.07874015748031495954, 0.07475334604056275978 ) ) ;
#9058 = FACE_OUTER_BOUND ( 'NONE', #904, .T. ) ;
#9059 = CARTESIAN_POINT ( 'NONE',  ( -0.09842519685028340570, -0.09842519685039370636, -0.5909884645248143498 ) ) ;
#9060 = EDGE_LOOP ( 'NONE', ( #2744, #11778, #1654, #3551, #9495 ) ) ;
#9061 = VERTEX_POINT ( 'NONE', #13830 ) ;
#9062 = ORIENTED_EDGE ( 'NONE', *, *, #11927, .F. ) ;
#9063 = ORIENTED_EDGE ( 'NONE', *, *, #13355, .T. ) ;
#9064 = AXIS2_PLACEMENT_3D ( 'NONE', #10456, #15236, #1996 ) ;
#9065 = EDGE_CURVE ( 'NONE', #2195, #10501, #12414, .T. ) ;
#9066 = CARTESIAN_POINT ( 'NONE',  ( -0.1629063847838169987, -0.1023622047244094474, 0.2161887458866224576 ) ) ;
#9067 = CARTESIAN_POINT ( 'NONE',  ( 0.7455328141524918406, 1.338582677165354395, 0.3622425942646915753 ) ) ;
#9068 = ADVANCED_FACE ( 'NONE', ( #15174 ), #7476, .T. ) ;
#9069 = DIRECTION ( 'NONE',  ( -1.000000000000000000, -0.000000000000000000, -3.476578583725179813E-16 ) ) ;
#9070 = CARTESIAN_POINT ( 'NONE',  ( -0.05114323250695500950, 0.05905511811023622659, 0.08858267716535433989 ) ) ;
#9071 = ADVANCED_FACE ( 'NONE', ( #528, #759 ), #7650, .F. ) ;
#9072 = CARTESIAN_POINT ( 'NONE',  ( -0.5860051159906336515, 0.000000000000000000, 0.1591122789105256508 ) ) ;
#9073 = FACE_OUTER_BOUND ( 'NONE', #12784, .T. ) ;
#9074 = CARTESIAN_POINT ( 'NONE',  ( -1.924914443801520880, -2.804978272008806339, -0.1525920034357165223 ) ) ;
#9075 = ORIENTED_EDGE ( 'NONE', *, *, #750, .F. ) ;
#9076 = DIRECTION ( 'NONE',  ( 0.000000000000000000, 0.000000000000000000, 1.000000000000000000 ) ) ;
#9077 = ORIENTED_EDGE ( 'NONE', *, *, #5318, .F. ) ;
#9078 =( BOUNDED_SURFACE ( )  B_SPLINE_SURFACE ( 3, 2, ( 
 ( #4643, #9435, #10748 ),
 ( #14207, #4784, #5882 ),
 ( #14347, #13184, #2448 ),
 ( #3704, #6024, #15462 ),
 ( #98, #4724, #13253 ),
 ( #4864, #8478, #9508 ),
 ( #14276, #3541, #8112 ),
 ( #8337, #2243, #4582 ),
 ( #14235, #10470, #13994 ),
 ( #13046, #12899, #8030 ) ),
 .UNSPECIFIED., .F., .F., .T. ) 
 B_SPLINE_SURFACE_WITH_KNOTS ( ( 4, 2, 2, 2, 4 ),
 ( 3, 3 ),
 ( -4.336808689942017736E-19, 0.0004011410879367268431, 0.0008022821758734541200, 0.001203423263810181505, 0.001604564351746908674 ),
 ( 0.000000000000000000, 1.000000000000000000 ),
 .UNSPECIFIED. ) 
 GEOMETRIC_REPRESENTATION_ITEM ( )  RATIONAL_B_SPLINE_SURFACE ( (
 ( 1.000000000000000000, 0.6273322353868007184, 1.000000000000000000),
 ( 1.000000000000000000, 0.6273746451327694151, 1.000000000000000000),
 ( 1.000000000000000000, 0.6276600930324378602, 1.000000000000000000),
 ( 1.000000000000000000, 0.6305495266240448426, 1.000000000000000000),
 ( 1.000000000000000000, 0.6332412771137517771, 1.000000000000000000),
 ( 1.000000000000000000, 0.6440211513203998317, 1.000000000000000000),
 ( 1.000000000000000000, 0.6523247361999675586, 1.000000000000000000),
 ( 1.000000000000000000, 0.6753292279000220333, 1.000000000000000000),
 ( 1.000000000000000000, 0.6902147318493536687, 1.000000000000000000),
 ( 1.000000000000000000, 0.7071067811865465735, 1.000000000000000000) ) ) 
 REPRESENTATION_ITEM ( '' )  SURFACE ( )  );
#9079 = ORIENTED_EDGE ( 'NONE', *, *, #6701, .T. ) ;
#9080 = UNCERTAINTY_MEASURE_WITH_UNIT (LENGTH_MEASURE( 1.000000000000000082E-05 ), #10155, 'distance_accuracy_value', 'NONE');
#9081 = ORIENTED_EDGE ( 'NONE', *, *, #9306, .F. ) ;
#9082 = CIRCLE ( 'NONE', #13831, 0.01968503937007883009 ) ;
#9083 = DIRECTION ( 'NONE',  ( -3.476578583725179813E-16, -0.000000000000000000, 1.000000000000000000 ) ) ;
#9084 = AXIS2_PLACEMENT_3D ( 'NONE', #14486, #13292, #7417 ) ;
#9085 = CIRCLE ( 'NONE', #15351, 0.03937007874015751446 ) ;
#9086 = CARTESIAN_POINT ( 'NONE',  ( -0.4121618538092056139, -0.2952755905511811330, 0.1243101294532692330 ) ) ;
#9087 = FACE_OUTER_BOUND ( 'NONE', #2730, .T. ) ;
#9088 = DIRECTION ( 'NONE',  ( 0.5801894994542535766, 0.8144815189573197944, 0.000000000000000000 ) ) ;
#9089 = DIRECTION ( 'NONE',  ( 0.000000000000000000, 0.000000000000000000, -1.000000000000000000 ) ) ;
#9090 = CARTESIAN_POINT ( 'NONE',  ( 0.000000000000000000, -0.4921259842519685179, 0.000000000000000000 ) ) ;
#9091 = EDGE_LOOP ( 'NONE', ( #111, #635 ) ) ;
#9092 = CARTESIAN_POINT ( 'NONE',  ( 0.06692913385832206796, -0.4921259842519685179, 9.675294977568793108E-18 ) ) ;
#9093 = CARTESIAN_POINT ( 'NONE',  ( 0.000000000000000000, 0.3228346456692913757, 0.7007874015748031260 ) ) ;
#9094 = CIRCLE ( 'NONE', #8341, 0.5433070866141731514 ) ;
#9095 = CARTESIAN_POINT ( 'NONE',  ( 0.05905511811023622659, 1.190944881889763884, -0.7874015748031497619 ) ) ;
#9096 = DIRECTION ( 'NONE',  ( 0.5000000000000134337, 0.000000000000000000, -0.8660254037844308250 ) ) ;
#9097 = ORIENTED_EDGE ( 'NONE', *, *, #7823, .F. ) ;
#9098 = CIRCLE ( 'NONE', #10846, 0.01968503937007873988 ) ;
#9099 = CARTESIAN_POINT ( 'NONE',  ( -0.5418660417173573052, -0.1023622047244094474, 0.2355633981508970798 ) ) ;
#9100 = VECTOR ( 'NONE', #1807, 39.37007874015748854 ) ;
#9101 = ORIENTED_EDGE ( 'NONE', *, *, #13171, .F. ) ;
#9102 = ORIENTED_EDGE ( 'NONE', *, *, #8442, .T. ) ;
#9103 = ORIENTED_EDGE ( 'NONE', *, *, #8119, .F. ) ;
#9104 = DIRECTION ( 'NONE',  ( -0.8660254037844385966, 0.000000000000000000, -0.5000000000000001110 ) ) ;
#9105 = DIRECTION ( 'NONE',  ( 0.000000000000000000, -0.000000000000000000, 1.000000000000000000 ) ) ;
#9106 = AXIS2_PLACEMENT_3D ( 'NONE', #7719, #2775, #11308 ) ;
#9107 = CIRCLE ( 'NONE', #2845, 0.003937007874015749712 ) ;
#9108 = EDGE_CURVE ( 'NONE', #5548, #8918, #4398, .T. ) ;
#9109 = AXIS2_PLACEMENT_3D ( 'NONE', #6355, #8797, #12263 ) ;
#9110 = CARTESIAN_POINT ( 'NONE',  ( -0.1618514667033796040, -0.4921259842519685179, 0.2161887458866224576 ) ) ;
#9111 = DIRECTION ( 'NONE',  ( -0.8660254037844398178, 0.000000000000000000, 0.4999999999999979461 ) ) ;
#9112 = CIRCLE ( 'NONE', #7850, 0.1574803149606299191 ) ;
#9113 = DIRECTION ( 'NONE',  ( 1.000000000000000000, 0.000000000000000000, 0.000000000000000000 ) ) ;
#9114 = CIRCLE ( 'NONE', #12128, 0.003937007874015749712 ) ;
#9115 = EDGE_CURVE ( 'NONE', #1223, #7284, #13692, .T. ) ;
#9116 = CARTESIAN_POINT ( 'NONE',  ( -0.06425120930260368179, -0.1863186860285575841, 0.03845354371037630614 ) ) ;
#9117 = ORIENTED_EDGE ( 'NONE', *, *, #13508, .T. ) ;
#9118 = DIRECTION ( 'NONE',  ( 0.8660254037844363761, 0.000000000000000000, -0.5000000000000038858 ) ) ;
#9119 = MANIFOLD_SOLID_BREP ( 'Fillet1', #3375 ) ;
#9120 = CARTESIAN_POINT ( 'NONE',  ( 0.3944453183761336135, -0.2952755905511811330, 0.1549960689574419737 ) ) ;
#9121 = EDGE_CURVE ( 'NONE', #12971, #12485, #14163, .T. ) ;
#9122 = CYLINDRICAL_SURFACE ( 'NONE', #12185, 2.214566929133857887 ) ;
#9123 = ORIENTED_EDGE ( 'NONE', *, *, #9231, .F. ) ;
#9124 = AXIS2_PLACEMENT_3D ( 'NONE', #767, #3121, #12758 ) ;
#9125 = AXIS2_PLACEMENT_3D ( 'NONE', #11558, #6940, #12812 ) ;
#9126 = AXIS2_PLACEMENT_3D ( 'NONE', #1883, #7911, #2026 ) ;
#9127 = ORIENTED_EDGE ( 'NONE', *, *, #11927, .T. ) ;
#9128 = VECTOR ( 'NONE', #7120, 39.37007874015748143 ) ;
#9129 = DIRECTION ( 'NONE',  ( 0.000000000000000000, 1.000000000000000000, 0.000000000000000000 ) ) ;
#9130 = ORIENTED_EDGE ( 'NONE', *, *, #708, .F. ) ;
#9131 = AXIS2_PLACEMENT_3D ( 'NONE', #1432, #2676, #5161 ) ;
#9132 = EDGE_LOOP ( 'NONE', ( #9063, #10058, #4924, #9994, #10227 ) ) ;
#9133 = ADVANCED_FACE ( 'NONE', ( #2307 ), #6852, .T. ) ;
#9134 = LINE ( 'NONE', #4427, #6848 ) ;
#9135 = FACE_OUTER_BOUND ( 'NONE', #7925, .T. ) ;
#9136 = AXIS2_PLACEMENT_3D ( 'NONE', #7856, #3080, #5429 ) ;
#9137 = EDGE_CURVE ( 'NONE', #12044, #10896, #4903, .T. ) ;
#9138 = DIRECTION ( 'NONE',  ( 0.000000000000000000, 0.000000000000000000, -1.000000000000000000 ) ) ;
#9139 = CIRCLE ( 'NONE', #2375, 0.003937007874015750579 ) ;
#9140 = DIRECTION ( 'NONE',  ( -0.000000000000000000, -1.000000000000000000, -0.000000000000000000 ) ) ;
#9141 = AXIS2_PLACEMENT_3D ( 'NONE', #4821, #12211, #8443 ) ;
#9142 = DIRECTION ( 'NONE',  ( 0.000000000000000000, 0.000000000000000000, 1.000000000000000000 ) ) ;
#9143 = EDGE_CURVE ( 'NONE', #13968, #14556, #11666, .T. ) ;
#9144 = DIRECTION ( 'NONE',  ( 0.000000000000000000, -1.000000000000000000, -0.000000000000000000 ) ) ;
#9145 = CARTESIAN_POINT ( 'NONE',  ( -1.946192867917151181, -2.743611295743891620, -0.1749236412511689931 ) ) ;
#9146 = EDGE_LOOP ( 'NONE', ( #12540, #7092 ) ) ;
#9147 = ORIENTED_EDGE ( 'NONE', *, *, #10888, .T. ) ;
#9148 = ORIENTED_EDGE ( 'NONE', *, *, #2177, .T. ) ;
#9149 = CIRCLE ( 'NONE', #5625, 3.169291338582677753 ) ;
#9150 = ORIENTED_EDGE ( 'NONE', *, *, #79, .F. ) ;
#9151 = CIRCLE ( 'NONE', #658, 0.03937007874015750752 ) ;
#9152 = CARTESIAN_POINT ( 'NONE',  ( -1.592432191550702480, 0.1184937169715563343, -0.04125010960116162056 ) ) ;
#9153 = DIRECTION ( 'NONE',  ( 0.5000000000000041078, -0.000000000000000000, 0.8660254037844363761 ) ) ;
#9154 = DIRECTION ( 'NONE',  ( -0.8660254037844383745, 0.000000000000000000, -0.5000000000000002220 ) ) ;
#9155 = DIRECTION ( 'NONE',  ( -1.000000000000000000, 0.000000000000000000, 0.000000000000000000 ) ) ;
#9156 = AXIS2_PLACEMENT_3D ( 'NONE', #13337, #5025, #6436 ) ;
#9157 = DIRECTION ( 'NONE',  ( -0.000000000000000000, -1.000000000000000000, -0.000000000000000000 ) ) ;
#9158 = PRESENTATION_LAYER_ASSIGNMENT (  '', '', ( #3661 ) ) ;
#9159 = CARTESIAN_POINT ( 'NONE',  ( -1.964126537190516997, -2.749515453455444014, -0.1756903148397123970 ) ) ;
#9160 = CIRCLE ( 'NONE', #7639, 0.2303149606299203511 ) ;
#9161 = VERTEX_POINT ( 'NONE', #4584 ) ;
#9162 = CARTESIAN_POINT ( 'NONE',  ( 7.232166136696967594E-17, 1.661417322834646049, 0.5905511811023621549 ) ) ;
#9163 = ADVANCED_FACE ( 'NONE', ( #14156 ), #4677, .T. ) ;
#9164 = DIRECTION ( 'NONE',  ( 1.000000000000000000, 0.000000000000000000, 3.614007241618343347E-16 ) ) ;
#9165 = EDGE_CURVE ( 'NONE', #7239, #7930, #14666, .T. ) ;
#9166 = PRODUCT_DEFINITION_SHAPE ( 'NONE', 'NONE',  #15493 ) ;
#9167 = VERTEX_POINT ( 'NONE', #8208 ) ;
#9168 = VERTEX_POINT ( 'NONE', #4749 ) ;
#9169 = EDGE_CURVE ( 'NONE', #13646, #2681, #5383, .T. ) ;
#9170 = ORIENTED_EDGE ( 'NONE', *, *, #8948, .T. ) ;
#9171 = CIRCLE ( 'NONE', #8666, 0.003937007874015724558 ) ;
#9172 = PLANE ( 'NONE',  #14644 ) ;
#9173 = DIRECTION ( 'NONE',  ( -0.000000000000000000, 0.000000000000000000, 1.000000000000000000 ) ) ;
#9174 = DIRECTION ( 'NONE',  ( 0.000000000000000000, 0.000000000000000000, 1.000000000000000000 ) ) ;
#9175 = DIRECTION ( 'NONE',  ( 0.000000000000000000, -0.000000000000000000, 1.000000000000000000 ) ) ;
#9176 = PLANE ( 'NONE',  #2632 ) ;
#9177 = ORIENTED_EDGE ( 'NONE', *, *, #1283, .F. ) ;
#9178 = CARTESIAN_POINT ( 'NONE',  ( 0.1618514667033794374, -0.4881889763779528324, 0.2083147301385909200 ) ) ;
#9179 = DIRECTION ( 'NONE',  ( 0.000000000000000000, 0.000000000000000000, -1.000000000000000000 ) ) ;
#9180 = MECHANICAL_DESIGN_GEOMETRIC_PRESENTATION_REPRESENTATION (  '', ( #8431 ), #932 ) ;
#9181 = CARTESIAN_POINT ( 'NONE',  ( 0.06351958502452506594, -0.4881889763779528324, -0.2357441700067326729 ) ) ;
#9182 = B_SPLINE_CURVE_WITH_KNOTS ( 'NONE', 3,
 ( #13490, #12394, #1572, #557, #5481, #1895, #6331, #11453 ),
 .UNSPECIFIED., .F., .F.,
 ( 4, 2, 2, 4 ),
 ( 0.005704847486038692669, 0.01714141318827901161, 0.02285969603939917022, 0.02857797889051934964 ),
 .UNSPECIFIED. ) ;
#9183 = ORIENTED_EDGE ( 'NONE', *, *, #14959, .F. ) ;
#9184 = PLANE ( 'NONE',  #3439 ) ;
#9185 = AXIS2_PLACEMENT_3D ( 'NONE', #87, #10663, #4846 ) ;
#9186 = VERTEX_POINT ( 'NONE', #3503 ) ;
#9187 = ADVANCED_FACE ( 'NONE', ( #10774 ), #14927, .T. ) ;
#9188 = ORIENTED_EDGE ( 'NONE', *, *, #3366, .T. ) ;
#9189 = ORIENTED_EDGE ( 'NONE', *, *, #1367, .T. ) ;
#9190 = DIRECTION ( 'NONE',  ( -0.8660254037844398178, 0.000000000000000000, 0.4999999999999979461 ) ) ;
#9191 = CIRCLE ( 'NONE', #9949, 3.149606299212599048 ) ;
#9192 = FACE_OUTER_BOUND ( 'NONE', #6181, .T. ) ;
#9193 = CARTESIAN_POINT ( 'NONE',  ( -0.4749369078591176851, -0.4881889763779528324, 0.3514880584999471314 ) ) ;
#9194 = CONTEXT_DEPENDENT_SHAPE_REPRESENTATION ( #10212, #3939 ) ;
#9195 = FACE_OUTER_BOUND ( 'NONE', #12768, .T. ) ;
#9196 = CIRCLE ( 'NONE', #12200, 0.01968503937007875723 ) ;
#9197 = CARTESIAN_POINT ( 'NONE',  ( -0.02018259705034725071, -0.1802452534892125813, 1.049219007154695292E-17 ) ) ;
#9198 = EDGE_LOOP ( 'NONE', ( #2290, #13861, #2064, #4718 ) ) ;
#9199 = DIRECTION ( 'NONE',  ( 0.000000000000000000, 2.212657494868377674E-16, 1.000000000000000000 ) ) ;
#9200 = AXIS2_PLACEMENT_3D ( 'NONE', #492, #1970, #9088 ) ;
#9201 = CARTESIAN_POINT ( 'NONE',  ( -1.580080891953810962, 0.1020406297922289152, 0.07529375917875073820 ) ) ;
#9202 = SURFACE_SIDE_STYLE ('',( #12876 ) ) ;
#9203 = CARTESIAN_POINT ( 'NONE',  ( 0.000000000000000000, 0.5826771653543306728, 0.000000000000000000 ) ) ;
#9204 = VERTEX_POINT ( 'NONE', #10706 ) ;
#9205 = AXIS2_PLACEMENT_3D ( 'NONE', #12390, #14752, #13549 ) ;
#9206 = ORIENTED_EDGE ( 'NONE', *, *, #8948, .F. ) ;
#9207 = APPLICATION_CONTEXT ( 'automotive_design' ) ;
#9208 = DIRECTION ( 'NONE',  ( -0.8660254037844385966, 0.000000000000000000, -0.5000000000000001110 ) ) ;
#9209 = EDGE_LOOP ( 'NONE', ( #10869, #2708, #3554, #6341 ) ) ;
#9210 = AXIS2_PLACEMENT_3D ( 'NONE', #4563, #9350, #8185 ) ;
#9211 = ADVANCED_FACE ( 'NONE', ( #13048 ), #7085, .T. ) ;
#9212 = VERTEX_POINT ( 'NONE', #9536 ) ;
#9213 = ADVANCED_FACE ( 'NONE', ( #14305 ), #13997, .F. ) ;
#9214 = LINE ( 'NONE', #3180, #7097 ) ;
#9215 = DIRECTION ( 'NONE',  ( -0.5000000000000039968, 0.000000000000000000, -0.8660254037844362651 ) ) ;
#9216 = AXIS2_PLACEMENT_3D ( 'NONE', #1736, #7366, #10981 ) ;
#9217 = DIRECTION ( 'NONE',  ( -0.8660254037844432595, 0.000000000000000000, -0.4999999999999918954 ) ) ;
#9218 = CARTESIAN_POINT ( 'NONE',  ( -1.574484809660005480, 0.1100025355994808662, -0.06175692796176408816 ) ) ;
#9219 = DIRECTION ( 'NONE',  ( -0.000000000000000000, -0.000000000000000000, 1.000000000000000000 ) ) ;
#9220 = AXIS2_PLACEMENT_3D ( 'NONE', #14622, #2483, #14477 ) ;
#9221 = DIRECTION ( 'NONE',  ( 1.000000000000000000, 0.000000000000000000, -1.224646799147353207E-16 ) ) ;
#9222 = DIRECTION ( 'NONE',  ( -1.000000000000000000, 0.000000000000000000, -0.000000000000000000 ) ) ;
#9223 = ORIENTED_EDGE ( 'NONE', *, *, #2756, .F. ) ;
#9224 = B_SPLINE_CURVE_WITH_KNOTS ( 'NONE', 3,
 ( #1410, #10795, #78, #2560, #9639, #6167 ),
 .UNSPECIFIED., .F., .F.,
 ( 4, 2, 4 ),
 ( 0.000000000000000000, 0.01440388436194928005, 0.02880776872389856011 ),
 .UNSPECIFIED. ) ;
#9225 = EDGE_LOOP ( 'NONE', ( #4440, #10952, #3846, #15365 ) ) ;
#9226 = EDGE_CURVE ( 'NONE', #13359, #6772, #7401, .T. ) ;
#9227 = VECTOR ( 'NONE', #12459, 39.37007874015748143 ) ;
#9228 = VERTEX_POINT ( 'NONE', #9832 ) ;
#9229 = ADVANCED_FACE ( 'NONE', ( #136 ), #9601, .T. ) ;
#9230 = ORIENTED_EDGE ( 'NONE', *, *, #11755, .F. ) ;
#9231 = EDGE_CURVE ( 'NONE', #12221, #10241, #9171, .T. ) ;
#9232 = CARTESIAN_POINT ( 'NONE',  ( -1.568343923620152847, 0.1178486908565804514, 0.05905511811023622659 ) ) ;
#9233 = CARTESIAN_POINT ( 'NONE',  ( -0.1023622047242991467, -0.4881889763779528324, -0.5909884645248143498 ) ) ;
#9234 = CARTESIAN_POINT ( 'NONE',  ( -0.008695292838828817469, 0.1754324108223994649, 0.01747077667448701521 ) ) ;
#9235 = DIRECTION ( 'NONE',  ( 0.000000000000000000, 0.000000000000000000, -1.000000000000000000 ) ) ;
#9236 = CARTESIAN_POINT ( 'NONE',  ( -0.008240795940610761566, -0.1611877539686306926, -0.01644599795625024952 ) ) ;
#9237 = CARTESIAN_POINT ( 'NONE',  ( -0.4822834645669303311, -0.09448818897637796532, 0.3466374647693610811 ) ) ;
#9238 = CARTESIAN_POINT ( 'NONE',  ( -1.949180757224311611, -2.798430349193752775, -0.1753397919474670996 ) ) ;
#9239 = ORIENTED_EDGE ( 'NONE', *, *, #15058, .T. ) ;
#9240 = DIRECTION ( 'NONE',  ( 0.000000000000000000, 0.000000000000000000, 1.000000000000000000 ) ) ;
#9241 = ORIENTED_EDGE ( 'NONE', *, *, #13719, .F. ) ;
#9242 = ORIENTED_EDGE ( 'NONE', *, *, #4575, .T. ) ;
#9243 = ADVANCED_FACE ( 'NONE', ( #12196, #219 ), #8661, .F. ) ;
#9244 = ORIENTED_EDGE ( 'NONE', *, *, #7804, .T. ) ;
#9245 = DIRECTION ( 'NONE',  ( 0.4999999999999998335, -0.000000000000000000, 0.8660254037844388186 ) ) ;
#9246 = EDGE_CURVE ( 'NONE', #14775, #11240, #3656, .T. ) ;
#9247 = CARTESIAN_POINT ( 'NONE',  ( -0.1531294576120625639, -0.4881889763779528324, -0.08840933357318579711 ) ) ;
#9248 = CARTESIAN_POINT ( 'NONE',  ( -1.927187694266953466, -2.943580729745926661, 0.04691452208654782463 ) ) ;
#9249 = DIRECTION ( 'NONE',  ( 1.000000000000000000, 0.000000000000000000, 0.000000000000000000 ) ) ;
#9250 = CARTESIAN_POINT ( 'NONE',  ( -2.090051324975654268, -1.858423098536573503, -0.08664193191035729491 ) ) ;
#9251 = CARTESIAN_POINT ( 'NONE',  ( 0.000000000000000000, 0.06496062992125986590, 0.000000000000000000 ) ) ;
#9252 = ORIENTED_EDGE ( 'NONE', *, *, #5257, .F. ) ;
#9253 = DIRECTION ( 'NONE',  ( -0.000000000000000000, -0.000000000000000000, -1.000000000000000000 ) ) ;
#9254 = EDGE_CURVE ( 'NONE', #3213, #13283, #7910, .T. ) ;
#9255 = LINE ( 'NONE', #6656, #14110 ) ;
#9256 = DIRECTION ( 'NONE',  ( 0.8660254037844491437, 0.000000000000000000, 0.4999999999999815148 ) ) ;
#9257 = DIRECTION ( 'NONE',  ( -0.000000000000000000, 1.000000000000000000, 0.000000000000000000 ) ) ;
#9258 = EDGE_LOOP ( 'NONE', ( #3908, #13401, #12223, #14316 ) ) ;
#9259 = CYLINDRICAL_SURFACE ( 'NONE', #12208, 0.007874015748031499423 ) ;
#9260 = ORIENTED_EDGE ( 'NONE', *, *, #11338, .F. ) ;
#9261 = VERTEX_POINT ( 'NONE', #1460 ) ;
#9262 = ORIENTED_EDGE ( 'NONE', *, *, #252, .T. ) ;
#9263 = EDGE_CURVE ( 'NONE', #6899, #4570, #4410, .T. ) ;
#9264 = DIRECTION ( 'NONE',  ( -0.8660254037844395958, 0.000000000000000000, 0.4999999999999986122 ) ) ;
#9265 = CARTESIAN_POINT ( 'NONE',  ( -0.002500327830562678200, 0.1532658568795227105, 0.000000000000000000 ) ) ;
#9266 = CARTESIAN_POINT ( 'NONE',  ( 0.000000000000000000, 0.03149606299212599769, 0.000000000000000000 ) ) ;
#9267 = FACE_OUTER_BOUND ( 'NONE', #543, .T. ) ;
#9268 = CARTESIAN_POINT ( 'NONE',  ( -0.09842519685028340570, -0.4881889763779528324, -0.5870514566507987197 ) ) ;
#9269 = DIRECTION ( 'NONE',  ( -3.942553354492736135E-16, 0.000000000000000000, 1.000000000000000000 ) ) ;
#9270 = EDGE_CURVE ( 'NONE', #10323, #3491, #2917, .T. ) ;
#9271 = VERTEX_POINT ( 'NONE', #12267 ) ;
#9272 = CARTESIAN_POINT ( 'NONE',  ( -0.1618514667033796040, -0.4881889763779528324, 0.2161887458866224576 ) ) ;
#9273 = EDGE_CURVE ( 'NONE', #715, #4548, #666, .T. ) ;
#9274 = DIRECTION ( 'NONE',  ( 0.000000000000000000, 0.000000000000000000, 1.000000000000000000 ) ) ;
#9275 = DIRECTION ( 'NONE',  ( 1.000000000000000000, -0.000000000000000000, -0.000000000000000000 ) ) ;
#9276 = CARTESIAN_POINT ( 'NONE',  ( 0.4815353412745266848, 1.041793866378536437, 0.3474236500605469291 ) ) ;
#9277 =( NAMED_UNIT ( * ) SI_UNIT ( $, .STERADIAN. ) SOLID_ANGLE_UNIT ( ) );
#9278 = ORIENTED_EDGE ( 'NONE', *, *, #10742, .F. ) ;
#9279 = ORIENTED_EDGE ( 'NONE', *, *, #1071, .T. ) ;
#9280 = CARTESIAN_POINT ( 'NONE',  ( 0.5450083523900213223, 1.043307086614173373, 0.2464697422870267274 ) ) ;
#9281 = ORIENTED_EDGE ( 'NONE', *, *, #14895, .F. ) ;
#9282 = ORIENTED_EDGE ( 'NONE', *, *, #7775, .T. ) ;
#9283 = ORIENTED_EDGE ( 'NONE', *, *, #9520, .T. ) ;
#9284 = CARTESIAN_POINT ( 'NONE',  ( -1.115439883890946726, -0.06270839865334709717, -0.03937007874015747977 ) ) ;
#9285 = CARTESIAN_POINT ( 'NONE',  ( 0.2359202325322792559, -0.1023622047244094474, 0.06286251073447048088 ) ) ;
#9286 = CARTESIAN_POINT ( 'NONE',  ( -1.898327483181569963, -2.948264329531598893, 0.02398964596264746910 ) ) ;
#9287 = PRODUCT_DEFINITION_SHAPE ( 'NONE', 'NONE',  #15472 ) ;
#9288 = FACE_OUTER_BOUND ( 'NONE', #9802, .T. ) ;
#9289 = CARTESIAN_POINT ( 'NONE',  ( -1.100415514366371195, -0.04998955061625851709, 0.03937007874015747977 ) ) ;
#9290 = DIRECTION ( 'NONE',  ( 0.000000000000000000, 1.000000000000000000, 0.000000000000000000 ) ) ;
#9291 = DIRECTION ( 'NONE',  ( -0.000000000000000000, -1.000000000000000000, -0.000000000000000000 ) ) ;
#9292 =( CONVERSION_BASED_UNIT ( 'INCH', #12984 ) LENGTH_UNIT ( ) NAMED_UNIT ( #72 ) );
#9293 = EDGE_LOOP ( 'NONE', ( #4940, #4291, #15179, #13422 ) ) ;
#9294 = EDGE_LOOP ( 'NONE', ( #3803, #13489, #2558, #12553 ) ) ;
#9295 = EDGE_LOOP ( 'NONE', ( #10806, #5870, #1980, #3234 ) ) ;
#9296 = VERTEX_POINT ( 'NONE', #6277 ) ;
#9297 = DIRECTION ( 'NONE',  ( -0.000000000000000000, -0.000000000000000000, -1.000000000000000000 ) ) ;
#9298 = LINE ( 'NONE', #14072, #14888 ) ;
#9299 = CARTESIAN_POINT ( 'NONE',  ( -0.1022864650139100884, 0.000000000000000000, -1.048351444896847144E-20 ) ) ;
#9300 = CARTESIAN_POINT ( 'NONE',  ( -0.05175539059627463218, 0.07874015748031495954, 0.07475334604056275978 ) ) ;
#9301 = ADVANCED_FACE ( 'NONE', ( #14700 ), #10928, .T. ) ;
#9302 = DIRECTION ( 'NONE',  ( 0.000000000000000000, 0.000000000000000000, 1.000000000000000000 ) ) ;
#9303 = PLANE ( 'NONE',  #3395 ) ;
#9304 = DIRECTION ( 'NONE',  ( 0.000000000000000000, 0.000000000000000000, 1.000000000000000000 ) ) ;
#9305 = CYLINDRICAL_SURFACE ( 'NONE', #637, 0.003937007874015721089 ) ;
#9306 = EDGE_CURVE ( 'NONE', #5700, #2543, #999, .T. ) ;
#9307 = EDGE_LOOP ( 'NONE', ( #13820, #8821, #10397, #8045 ) ) ;
#9308 = DIRECTION ( 'NONE',  ( 0.000000000000000000, 0.000000000000000000, -1.000000000000000000 ) ) ;
#9309 = CARTESIAN_POINT ( 'NONE',  ( 0.1540707661268329032, 0.000000000000000000, -0.5890199605878065903 ) ) ;
#9310 = CARTESIAN_POINT ( 'NONE',  ( 0.000000000000000000, 0.3149606299212598381, 0.000000000000000000 ) ) ;
#9311 = ORIENTED_EDGE ( 'NONE', *, *, #14570, .T. ) ;
#9312 = ADVANCED_FACE ( 'NONE', ( #12330 ), #13439, .F. ) ;
#9313 = EDGE_LOOP ( 'NONE', ( #9102, #3208, #5199, #11024 ) ) ;
#9314 = ORIENTED_EDGE ( 'NONE', *, *, #14807, .F. ) ;
#9315 = FACE_BOUND ( 'NONE', #1384, .T. ) ;
#9316 = EDGE_CURVE ( 'NONE', #11599, #13144, #10670, .T. ) ;
#9317 = CARTESIAN_POINT ( 'NONE',  ( 1.976792077363838002E-17, -0.09842519685039370636, 0.1614173228346456879 ) ) ;
#9318 = CARTESIAN_POINT ( 'NONE',  ( -1.925470963062591023, -2.948261428410166918, -0.02401791239041710727 ) ) ;
#9319 = CARTESIAN_POINT ( 'NONE',  ( 0.1062992125984796032, -0.4881889763779528324, -0.2482618547481154347 ) ) ;
#9320 = DIRECTION ( 'NONE',  ( 0.000000000000000000, 0.000000000000000000, 1.000000000000000000 ) ) ;
#9321 = CARTESIAN_POINT ( 'NONE',  ( -1.190198933766848155, 0.3259758027579586215, -0.05905511811023622659 ) ) ;
#9322 = EDGE_CURVE ( 'NONE', #8997, #5195, #15176, .T. ) ;
#9323 = ORIENTED_EDGE ( 'NONE', *, *, #9610, .F. ) ;
#9324 = CARTESIAN_POINT ( 'NONE',  ( 0.4552518684890383138, -0.1023622047244094474, 0.3855835468379170128 ) ) ;
#9325 = CARTESIAN_POINT ( 'NONE',  ( -0.4751993499419962519, 1.035433070866141891, 0.3506226965216301950 ) ) ;
#9326 = DIRECTION ( 'NONE',  ( 0.000000000000000000, -8.673617379884032317E-15, 1.000000000000000000 ) ) ;
#9327 = ORIENTED_EDGE ( 'NONE', *, *, #5501, .F. ) ;
#9328 = EDGE_CURVE ( 'NONE', #14956, #1166, #11161, .T. ) ;
#9329 = CYLINDRICAL_SURFACE ( 'NONE', #1690, 0.1574803149606299191 ) ;
#9330 = VECTOR ( 'NONE', #9706, 39.37007874015748143 ) ;
#9331 = EDGE_LOOP ( 'NONE', ( #13770, #7109, #12020, #12470 ) ) ;
#9332 = CIRCLE ( 'NONE', #10582, 0.5511811023622046335 ) ;
#9333 = ORIENTED_EDGE ( 'NONE', *, *, #277, .F. ) ;
#9334 = ORIENTED_EDGE ( 'NONE', *, *, #4999, .T. ) ;
#9335 = ORIENTED_EDGE ( 'NONE', *, *, #2623, .T. ) ;
#9336 = CARTESIAN_POINT ( 'NONE',  ( 0.1552072824047652788, 0.000000000000000000, -0.5870514566507987197 ) ) ;
#9337 = DIRECTION ( 'NONE',  ( 4.336808689942014285E-16, 0.000000000000000000, -1.000000000000000000 ) ) ;
#9338 = DIRECTION ( 'NONE',  ( 1.000000000000000000, -0.000000000000000000, -0.000000000000000000 ) ) ;
#9339 = DIRECTION ( 'NONE',  ( 0.000000000000000000, 0.000000000000000000, 1.000000000000000000 ) ) ;
#9340 = ITEM_DEFINED_TRANSFORMATION ( 'NONE', 'NONE', #10125,  #11481 ) ;
#9341 = DIRECTION ( 'NONE',  ( 0.000000000000000000, 0.000000000000000000, -1.000000000000000000 ) ) ;
#9342 = VECTOR ( 'NONE', #14509, 39.37007874015748143 ) ;
#9343 = AXIS2_PLACEMENT_3D ( 'NONE', #14715, #6463, #8812 ) ;
#9344 = CARTESIAN_POINT ( 'NONE',  ( -0.4330708661417336236, -0.09842519685039370636, 0.4318761856142863120 ) ) ;
#9345 = ORIENTED_EDGE ( 'NONE', *, *, #8407, .T. ) ;
#9346 = DIRECTION ( 'NONE',  ( 0.000000000000000000, 0.000000000000000000, 1.000000000000000000 ) ) ;
#9347 = CIRCLE ( 'NONE', #11085, 0.5905511811023621549 ) ;
#9348 = VECTOR ( 'NONE', #2973, 39.37007874015748143 ) ;
#9349 = LINE ( 'NONE', #11622, #7873 ) ;
#9350 = DIRECTION ( 'NONE',  ( -1.000000000000000000, -0.000000000000000000, -0.000000000000000000 ) ) ;
#9351 = DIRECTION ( 'NONE',  ( -0.8660254037844387076, 0.000000000000000000, -0.4999999999999998890 ) ) ;
#9352 = EDGE_CURVE ( 'NONE', #13856, #12057, #1380, .T. ) ;
#9353 = ORIENTED_EDGE ( 'NONE', *, *, #15367, .T. ) ;
#9354 = VERTEX_POINT ( 'NONE', #6364 ) ;
#9355 = B_SPLINE_CURVE_WITH_KNOTS ( 'NONE', 3,
 ( #2978, #10024, #8940, #5468 ),
 .UNSPECIFIED., .F., .F.,
 ( 4, 4 ),
 ( 0.000000000000000000, 2.119993237936343888E-05 ),
 .UNSPECIFIED. ) ;
#9356 = DIRECTION ( 'NONE',  ( 0.000000000000000000, -1.000000000000000000, 2.212657494868377674E-16 ) ) ;
#9358 = VERTEX_POINT ( 'NONE', #15069 ) ;
#9357 = VECTOR ( 'NONE', #1696, 39.37007874015748854 ) ;
#9359 = AXIS2_PLACEMENT_3D ( 'NONE', #802, #8009, #3397 ) ;
#9360 = ORIENTED_EDGE ( 'NONE', *, *, #13331, .F. ) ;
#9361 = EDGE_CURVE ( 'NONE', #9837, #450, #3279, .T. ) ;
#9362 = EDGE_LOOP ( 'NONE', ( #9609, #5972, #10794, #7514 ) ) ;
#9363 = CIRCLE ( 'NONE', #13594, 0.01968503937007872948 ) ;
#9364 = FACE_OUTER_BOUND ( 'NONE', #6192, .T. ) ;
#9365 = DIRECTION ( 'NONE',  ( -0.5000000000000035527, -0.000000000000000000, 0.8660254037844365982 ) ) ;
#9366 = DIRECTION ( 'NONE',  ( 0.8660254037844384856, 0.000000000000000000, 0.5000000000000003331 ) ) ;
#9367 = CARTESIAN_POINT ( 'NONE',  ( -1.961853848035927994, -2.757152788027944279, -0.1766820469359192958 ) ) ;
#9368 = DIRECTION ( 'NONE',  ( 0.000000000000000000, -1.000000000000000000, 0.000000000000000000 ) ) ;
#9369 = CARTESIAN_POINT ( 'NONE',  ( -0.2393297813659119588, -0.1023622047244094474, 0.06089400679736759608 ) ) ;
#9370 = DIRECTION ( 'NONE',  ( 0.000000000000000000, -4.956352788505160310E-16, -1.000000000000000000 ) ) ;
#9371 = CIRCLE ( 'NONE', #4102, 0.003937007874015721089 ) ;
#9372 = VECTOR ( 'NONE', #2475, 39.37007874015748143 ) ;
#9373 = DIRECTION ( 'NONE',  ( -1.000000000000000000, 0.000000000000000000, 0.000000000000000000 ) ) ;
#9374 = CARTESIAN_POINT ( 'NONE',  ( 0.000000000000000000, -0.09842519685039370636, 0.000000000000000000 ) ) ;
#9375 = AXIS2_PLACEMENT_3D ( 'NONE', #14267, #5782, #8387 ) ;
#9376 = AXIS2_PLACEMENT_3D ( 'NONE', #5109, #6043, #8498 ) ;
#9377 = VERTEX_POINT ( 'NONE', #5260 ) ;
#9378 =( GEOMETRIC_REPRESENTATION_CONTEXT ( 3 ) GLOBAL_UNCERTAINTY_ASSIGNED_CONTEXT ( ( #1881 ) ) GLOBAL_UNIT_ASSIGNED_CONTEXT ( ( #1593, #6584, #11295 ) ) REPRESENTATION_CONTEXT ( 'NONE', 'WORKASPACE' ) );
#9379 = VERTEX_POINT ( 'NONE', #8979 ) ;
#9380 = ORIENTED_EDGE ( 'NONE', *, *, #12567, .F. ) ;
#9381 = ORIENTED_EDGE ( 'NONE', *, *, #3001, .F. ) ;
#9382 = PRODUCT_RELATED_PRODUCT_CATEGORY ( 'part', '', ( #8693 ) ) ;
#9383 = AXIS2_PLACEMENT_3D ( 'NONE', #5885, #5965, #7292 ) ;
#9384 = AXIS2_PLACEMENT_3D ( 'NONE', #3038, #12361, #6540 ) ;
#9385 = TOROIDAL_SURFACE ( 'NONE', #10142, 0.05905511811023621271, 0.01968503937007873988 ) ;
#9386 = AXIS2_PLACEMENT_3D ( 'NONE', #95, #1337, #11938 ) ;
#9387 = FACE_OUTER_BOUND ( 'NONE', #15468, .T. ) ;
#9388 = CIRCLE ( 'NONE', #13632, 0.003937007874015750579 ) ;
#9389 = CARTESIAN_POINT ( 'NONE',  ( -0.002322522588111503115, 0.1532890258252367910, -0.0007019553870510035357 ) ) ;
#9390 = CARTESIAN_POINT ( 'NONE',  ( -0.004688298860636734219, -0.1607931678657649743, -0.008473975361459462965 ) ) ;
#9391 = DIRECTION ( 'NONE',  ( -0.8660254037844389297, 0.000000000000000000, 0.4999999999999996114 ) ) ;
#9392 = DIRECTION ( 'NONE',  ( -1.000000000000000000, -0.000000000000000000, -3.973232667114495301E-16 ) ) ;
#9393 = VERTEX_POINT ( 'NONE', #7778 ) ;
#9394 = CARTESIAN_POINT ( 'NONE',  ( 0.09842519685044820443, -0.1023622047244094474, -0.5870514566507987197 ) ) ;
#9395 = PLANE ( 'NONE',  #5057 ) ;
#9396 = DIRECTION ( 'NONE',  ( 0.000000000000000000, 0.000000000000000000, -1.000000000000000000 ) ) ;
#9397 = TOROIDAL_SURFACE ( 'NONE', #15151, 0.04330708661417328326, 0.003937007874015747977 ) ;
#9398 = AXIS2_PLACEMENT_3D ( 'NONE', #4765, #9548, #8361 ) ;
#9399 = VECTOR ( 'NONE', #6008, 39.37007874015748143 ) ;
#9400 = ORIENTED_EDGE ( 'NONE', *, *, #14062, .F. ) ;
#9401 = ORIENTED_EDGE ( 'NONE', *, *, #10840, .F. ) ;
#9402 = AXIS2_PLACEMENT_3D ( 'NONE', #14800, #12456, #11192 ) ;
#9403 = EDGE_CURVE ( 'NONE', #2172, #9995, #7663, .T. ) ;
#9404 = VERTEX_POINT ( 'NONE', #4325 ) ;
#9405 = ADVANCED_FACE ( 'NONE', ( #5193 ), #9122, .T. ) ;
#9406 = FACE_OUTER_BOUND ( 'NONE', #13049, .T. ) ;
#9407 = AXIS2_PLACEMENT_3D ( 'NONE', #11886, #7176, #8274 ) ;
#9408 = CIRCLE ( 'NONE', #8149, 0.003937007874015749712 ) ;
#9409 = ADVANCED_FACE ( 'NONE', ( #13751 ), #12737, .T. ) ;
#9410 = DIRECTION ( 'NONE',  ( 1.000000000000000000, 0.000000000000000000, 3.075191616504340279E-15 ) ) ;
#9411 = DIRECTION ( 'NONE',  ( -0.000000000000000000, -0.000000000000000000, -1.000000000000000000 ) ) ;
#9412 = DIRECTION ( 'NONE',  ( 0.000000000000000000, 1.000000000000000000, 0.000000000000000000 ) ) ;
#9413 = AXIS2_PLACEMENT_3D ( 'NONE', #2485, #14545, #14401 ) ;
#9414 = DIRECTION ( 'NONE',  ( 1.224646799147353454E-16, 0.000000000000000000, -1.000000000000000000 ) ) ;
#9415 = VERTEX_POINT ( 'NONE', #12422 ) ;
#9416 =( REPRESENTATION_RELATIONSHIP ('NONE','NONE', #8904, #7785 ) REPRESENTATION_RELATIONSHIP_WITH_TRANSFORMATION ( #4314 )SHAPE_REPRESENTATION_RELATIONSHIP( ) );
#9417 = CARTESIAN_POINT ( 'NONE',  ( -1.387704745771440207, -0.02010536753476152225, 0.03937007874015747977 ) ) ;
#9418 = CARTESIAN_POINT ( 'NONE',  ( -0.3137366569588388998, -0.2952755905511811330, 0.2947875711430708590 ) ) ;
#9419 = CARTESIAN_POINT ( 'NONE',  ( -0.2681506793016945611, -0.4881889763779528324, 0.03207310886158504931 ) ) ;
#9420 = CARTESIAN_POINT ( 'NONE',  ( -0.2373612774289040883, -0.4881889763779528324, 0.06430355563116459117 ) ) ;
#9421 = ORIENTED_EDGE ( 'NONE', *, *, #256, .F. ) ;
#9422 = DIRECTION ( 'NONE',  ( 0.000000000000000000, 0.000000000000000000, 1.000000000000000000 ) ) ;
#9423 = AXIS2_PLACEMENT_3D ( 'NONE', #1516, #13495, #13561 ) ;
#9424 = VECTOR ( 'NONE', #577, 39.37007874015748854 ) ;
#9425 = EDGE_LOOP ( 'NONE', ( #15451, #1763, #1403 ) ) ;
#9426 = ADVANCED_FACE ( 'NONE', ( #7946 ), #3671, .F. ) ;
#9427 = ORIENTED_EDGE ( 'NONE', *, *, #2802, .T. ) ;
#9428 = AXIS2_PLACEMENT_3D ( 'NONE', #4413, #2291, #195 ) ;
#9429 = EDGE_CURVE ( 'NONE', #9678, #5876, #1921, .T. ) ;
#9430 = PRODUCT_DEFINITION_SHAPE ( 'NONE', 'NONE',  #9773 ) ;
#9431 = VERTEX_POINT ( 'NONE', #10057 ) ;
#9432 = CARTESIAN_POINT ( 'NONE',  ( -1.992382107315057160, -2.749515453455444014, -0.1756903148397123138 ) ) ;
#9433 = DIRECTION ( 'NONE',  ( -1.000000000000000000, 0.000000000000000000, 0.000000000000000000 ) ) ;
#9434 = ADVANCED_FACE ( 'NONE', ( #14838 ), #7713, .T. ) ;
#9435 = CARTESIAN_POINT ( 'NONE',  ( -1.399712685227380016, -0.02644324263748132689, 0.07874015748031497341 ) ) ;
#9436 = DIRECTION ( 'NONE',  ( -0.4999999999999919509, 0.000000000000000000, 0.8660254037844432595 ) ) ;
#9437 = DIRECTION ( 'NONE',  ( -0.5000000000000008882, 0.000000000000000000, 0.8660254037844380415 ) ) ;
#9438 = AXIS2_PLACEMENT_3D ( 'NONE', #13557, #6340, #5245 ) ;
#9439 = CARTESIAN_POINT ( 'NONE',  ( -0.06299212598414166697, -0.2952755905511811330, -0.4190977005962941426 ) ) ;
#9440 = VERTEX_POINT ( 'NONE', #6681 ) ;
#9441 = CARTESIAN_POINT ( 'NONE',  ( -0.06299212598414161146, -0.4881889763779528324, -0.5870514566507987197 ) ) ;
#9442 = CARTESIAN_POINT ( 'NONE',  ( -1.580080891953811628, 0.1020406297922293454, 0.07874015748031495954 ) ) ;
#9443 = CARTESIAN_POINT ( 'NONE',  ( 0.6864776960422569463, 1.190944881889763884, 0.4645290592786023298 ) ) ;
#9444 = CARTESIAN_POINT ( 'NONE',  ( -0.4552518684890389244, -0.1023622047244094474, 0.3855835468379172903 ) ) ;
#9445 = AXIS2_PLACEMENT_3D ( 'NONE', #15063, #15145, #11616 ) ;
#9446 = VERTEX_POINT ( 'NONE', #6755 ) ;
#9447 = DIRECTION ( 'NONE',  ( 0.000000000000000000, 0.000000000000000000, -1.000000000000000000 ) ) ;
#9448 = VERTEX_POINT ( 'NONE', #674 ) ;
#9449 = VECTOR ( 'NONE', #13329, 39.37007874015748143 ) ;
#9450 = EDGE_CURVE ( 'NONE', #5709, #11465, #11394, .T. ) ;
#9451 = EDGE_LOOP ( 'NONE', ( #13000, #2965, #14591, #2342 ) ) ;
#9452 = EDGE_LOOP ( 'NONE', ( #11178, #9697, #15274, #6552 ) ) ;
#9453 = CARTESIAN_POINT ( 'NONE',  ( 0.06692913385832215123, -0.4881889763779528324, -0.5870514566507987197 ) ) ;
#9454 = VECTOR ( 'NONE', #8224, 39.37007874015748143 ) ;
#9455 = EDGE_CURVE ( 'NONE', #15013, #4047, #6515, .T. ) ;
#9456 = DIRECTION ( 'NONE',  ( 1.000000000000000000, 0.000000000000000000, 0.000000000000000000 ) ) ;
#9457 = CARTESIAN_POINT ( 'NONE',  ( -1.943208788703627787, -2.817317615915758466, -0.1717371570881610909 ) ) ;
#9458 =( CONVERSION_BASED_UNIT ( 'INCH', #5906 ) LENGTH_UNIT ( ) NAMED_UNIT ( #11877 ) );
#9459 = TOROIDAL_SURFACE ( 'NONE', #8947, 0.1240157480314959815, 0.003937007874015747977 ) ;
#9460 = SURFACE_SIDE_STYLE ('',( #4744 ) ) ;
#9461 = CYLINDRICAL_SURFACE ( 'NONE', #2896, 0.007874015748031516770 ) ;
#9462 = DIRECTION ( 'NONE',  ( 0.000000000000000000, -1.000000000000000000, 0.000000000000000000 ) ) ;
#9463 = CIRCLE ( 'NONE', #11450, 0.05905511811023620578 ) ;
#9464 = EDGE_CURVE ( 'NONE', #9877, #13444, #6591, .T. ) ;
#9465 = CARTESIAN_POINT ( 'NONE',  ( -0.5084014747882513729, -0.09842519685039370636, 0.2935257283253980276 ) ) ;
#9466 = CARTESIAN_POINT ( 'NONE',  ( 0.3706061991976989933, -0.003937007874015747977, -0.2139695888701345361 ) ) ;
#9467 = VECTOR ( 'NONE', #650, 39.37007874015748143 ) ;
#9468 = ORIENTED_EDGE ( 'NONE', *, *, #3363, .F. ) ;
#9469 = ORIENTED_EDGE ( 'NONE', *, *, #14593, .T. ) ;
#9470 = ORIENTED_EDGE ( 'NONE', *, *, #10361, .F. ) ;
#9471 = ORIENTED_EDGE ( 'NONE', *, *, #10874, .F. ) ;
#9472 = TOROIDAL_SURFACE ( 'NONE', #6183, 0.5984251968503937480, 0.007874015748031495954 ) ;
#9473 = FACE_OUTER_BOUND ( 'NONE', #14079, .T. ) ;
#9474 = CIRCLE ( 'NONE', #5446, 0.003937007874015724558 ) ;
#9475 = CARTESIAN_POINT ( 'NONE',  ( -2.182693454834259139, -1.630005269948474389, -0.08366141732283423338 ) ) ;
#9476 = CARTESIAN_POINT ( 'NONE',  ( -0.4606299212598433113, -0.4881889763779528324, 0.3841425019411278674 ) ) ;
#9477 = DIRECTION ( 'NONE',  ( 0.000000000000000000, 0.000000000000000000, -1.000000000000000000 ) ) ;
#9478 = DIRECTION ( 'NONE',  ( -0.8660254037844385966, 0.000000000000000000, -0.5000000000000001110 ) ) ;
#9479 = ORIENTED_EDGE ( 'NONE', *, *, #8348, .T. ) ;
#9480 = FILL_AREA_STYLE_COLOUR ( '', #14717 ) ;
#9481 = EDGE_CURVE ( 'NONE', #11443, #6019, #11545, .T. ) ;
#9482 = DIRECTION ( 'NONE',  ( 0.000000000000000000, -1.000000000000000000, 0.000000000000000000 ) ) ;
#9483 = LINE ( 'NONE', #3673, #10152 ) ;
#9484 = CIRCLE ( 'NONE', #7712, 0.007874015748031499423 ) ;
#9485 = ORIENTED_EDGE ( 'NONE', *, *, #5266, .T. ) ;
#9486 = ORIENTED_EDGE ( 'NONE', *, *, #12675, .T. ) ;
#9487 =( GEOMETRIC_REPRESENTATION_CONTEXT ( 3 ) GLOBAL_UNCERTAINTY_ASSIGNED_CONTEXT ( ( #12071 ) ) GLOBAL_UNIT_ASSIGNED_CONTEXT ( ( #14065, #1151, #13042 ) ) REPRESENTATION_CONTEXT ( 'NONE', 'WORKASPACE' ) );
#9488 = ORIENTED_EDGE ( 'NONE', *, *, #923, .F. ) ;
#9489 = DIRECTION ( 'NONE',  ( 0.000000000000000000, -0.000000000000000000, 1.000000000000000000 ) ) ;
#9490 = DIRECTION ( 'NONE',  ( -0.8660254037844385966, -0.000000000000000000, -0.5000000000000001110 ) ) ;
#9491 = CARTESIAN_POINT ( 'NONE',  ( 4.821444091131311524E-18, 0.4133858267716535306, 0.03937007874015747977 ) ) ;
#9492 = DIRECTION ( 'NONE',  ( 1.000000000000000000, -0.000000000000000000, 1.224646799147353207E-16 ) ) ;
#9493 = CARTESIAN_POINT ( 'NONE',  ( 0.000000000000000000, 2.637795275590551825, -0.03937007874015747977 ) ) ;
#9494 = CARTESIAN_POINT ( 'NONE',  ( -1.960454989549089699, -2.761853628972389174, 0.1772924660290619847 ) ) ;
#9495 = ORIENTED_EDGE ( 'NONE', *, *, #8684, .T. ) ;
#9496 = CARTESIAN_POINT ( 'NONE',  ( -1.959418227522675249, -2.897423706371843100, -0.1051064557059967070 ) ) ;
#9497 = CIRCLE ( 'NONE', #7236, 0.05298991407461853265 ) ;
#9498 = DIRECTION ( 'NONE',  ( -0.4999999999999998335, -0.000000000000000000, -0.8660254037844388186 ) ) ;
#9499 = CARTESIAN_POINT ( 'NONE',  ( -1.181102362204724310, -0.1240157480314959815, 0.02559055118110236185 ) ) ;
#9500 = CARTESIAN_POINT ( 'NONE',  ( 0.2742631158500650201, -0.2952755905511811330, 0.2765435766697818543 ) ) ;
#9501 = EDGE_LOOP ( 'NONE', ( #1834, #13799, #5217, #286 ) ) ;
#9502 = ORIENTED_EDGE ( 'NONE', *, *, #714, .T. ) ;
#9503 = EDGE_CURVE ( 'NONE', #4974, #5718, #4665, .T. ) ;
#9504 = VERTEX_POINT ( 'NONE', #14772 ) ;
#9505 = ORIENTED_EDGE ( 'NONE', *, *, #7324, .F. ) ;
#9506 = CARTESIAN_POINT ( 'NONE',  ( 0.1552072824047652788, -0.09448818897637796532, -0.5870514566507987197 ) ) ;
#9507 = DIRECTION ( 'NONE',  ( 0.8660254037844427044, 0.000000000000000000, 0.4999999999999928946 ) ) ;
#9508 = CARTESIAN_POINT ( 'NONE',  ( -1.411829724187707580, -0.008176884669458164834, 0.06280128582456272202 ) ) ;
#9509 = CARTESIAN_POINT ( 'NONE',  ( 1.137795275590550936, 4.097147066950659020E-16, 0.02952755905511811330 ) ) ;
#9510 = ITEM_DEFINED_TRANSFORMATION ( 'NONE', 'NONE', #2853,  #11481 ) ;
#9511 = DIRECTION ( 'NONE',  ( -0.000000000000000000, -1.000000000000000000, -0.000000000000000000 ) ) ;
#9512 = CARTESIAN_POINT ( 'NONE',  ( 0.1062992125984795477, -0.1023622047244094474, -0.2482618547481155458 ) ) ;
#9513 = VERTEX_POINT ( 'NONE', #10290 ) ;
#9514 = DIRECTION ( 'NONE',  ( 0.000000000000000000, 0.000000000000000000, 1.000000000000000000 ) ) ;
#9515 = DIRECTION ( 'NONE',  ( 0.5000000000000001110, 0.000000000000000000, -0.8660254037844385966 ) ) ;
#9516 = CARTESIAN_POINT ( 'NONE',  ( -0.04921259842516954863, -0.4921259842519685179, -0.08523872084487790768 ) ) ;
#9517 = EDGE_CURVE ( 'NONE', #288, #8683, #419, .T. ) ;
#9518 =( CONVERSION_BASED_UNIT ( 'INCH', #14132 ) LENGTH_UNIT ( ) NAMED_UNIT ( #10560 ) );
#9519 = EDGE_LOOP ( 'NONE', ( #4906, #3254, #11323, #2688 ) ) ;
#9520 = EDGE_CURVE ( 'NONE', #13891, #1499, #4163, .T. ) ;
#9521 = ORIENTED_EDGE ( 'NONE', *, *, #4904, .T. ) ;
#9522 = ORIENTED_EDGE ( 'NONE', *, *, #3073, .T. ) ;
#9523 = ORIENTED_EDGE ( 'NONE', *, *, #7700, .F. ) ;
#9524 = EDGE_LOOP ( 'NONE', ( #12334, #13335, #2846, #5294 ) ) ;
#9525 = DIRECTION ( 'NONE',  ( 0.000000000000000000, 0.000000000000000000, -1.000000000000000000 ) ) ;
#9526 = LINE ( 'NONE', #8497, #14364 ) ;
#9527 = CARTESIAN_POINT ( 'NONE',  ( 0.4307978335858662633, -0.09842519685039370636, 0.4279391777402732910 ) ) ;
#9528 = DIRECTION ( 'NONE',  ( -0.7118260687460302716, 0.5695655044020486724, -0.4109729724067160972 ) ) ;
#9529 = CARTESIAN_POINT ( 'NONE',  ( -0.2647411304678976007, -0.1023622047244094474, 0.03404161279859290595 ) ) ;
#9530 = EDGE_CURVE ( 'NONE', #9415, #5934, #12927, .T. ) ;
#9531 = DIRECTION ( 'NONE',  ( -0.8660254037844388186, 0.000000000000000000, 0.4999999999999995559 ) ) ;
#9532 = DIRECTION ( 'NONE',  ( -0.000000000000000000, -0.000000000000000000, 1.000000000000000000 ) ) ;
#9533 = CARTESIAN_POINT ( 'NONE',  ( -1.511943070284283097, 0.2262540267724839904, 0.03937007874015747977 ) ) ;
#9534 = EDGE_CURVE ( 'NONE', #10930, #2979, #6828, .T. ) ;
#9535 = DIRECTION ( 'NONE',  ( -0.000000000000000000, 0.000000000000000000, 1.000000000000000000 ) ) ;
#9536 = CARTESIAN_POINT ( 'NONE',  ( 0.1023622047244638067, -0.1023622047244094474, -0.2482618547481154347 ) ) ;
#9537 = EDGE_LOOP ( 'NONE', ( #2007, #7861, #248, #1090 ) ) ;
#9538 = EDGE_CURVE ( 'NONE', #9186, #12219, #15426, .T. ) ;
#9539 = EDGE_LOOP ( 'NONE', ( #8645, #7968, #140, #12801 ) ) ;
#9540 = VERTEX_POINT ( 'NONE', #5893 ) ;
#9541 = VERTEX_POINT ( 'NONE', #2058 ) ;
#9542 = DIRECTION ( 'NONE',  ( 0.000000000000000000, -0.000000000000000000, -1.000000000000000000 ) ) ;
#9543 = MANIFOLD_SOLID_BREP ( 'Fillet2', #8624 ) ;
#9544 = CARTESIAN_POINT ( 'NONE',  ( 0.9851651268172137987, -1.725292181286280480, 0.1968503937007874127 ) ) ;
#9545 = CARTESIAN_POINT ( 'NONE',  ( 0.000000000000000000, 0.4094488188976377896, 0.000000000000000000 ) ) ;
#9546 = ORIENTED_EDGE ( 'NONE', *, *, #10865, .T. ) ;
#9547 = CARTESIAN_POINT ( 'NONE',  ( 0.05114323250695499562, 0.05905511811023622659, -0.08858267716535433989 ) ) ;
#9548 = DIRECTION ( 'NONE',  ( 0.8660254037844400399, -2.152835902228474590E-14, -0.4999999999999977240 ) ) ;
#9549 = ORIENTED_EDGE ( 'NONE', *, *, #13446, .T. ) ;
#9550 = EDGE_LOOP ( 'NONE', ( #5489, #12521, #9546, #2816 ) ) ;
#9551 = EDGE_CURVE ( 'NONE', #2150, #8264, #3911, .T. ) ;
#9552 = ORIENTED_EDGE ( 'NONE', *, *, #9254, .F. ) ;
#9553 = EDGE_CURVE ( 'NONE', #11698, #2979, #11934, .T. ) ;
#9554 = CARTESIAN_POINT ( 'NONE',  ( 0.3964138223131414840, -0.2952755905511811330, 0.1515865201236449578 ) ) ;
#9555 = ADVANCED_FACE ( 'NONE', ( #2372 ), #12962, .T. ) ;
#9556 = CARTESIAN_POINT ( 'NONE',  ( -1.596214514713377719, 0.1135332889814021501, 0.07874015748031495954 ) ) ;
#9557 = CARTESIAN_POINT ( 'NONE',  ( -1.949533059518675726, -2.921996214527964764, -0.09505434699680524735 ) ) ;
#9558 = CARTESIAN_POINT ( 'NONE',  ( -0.5403775172679798899, 1.038795175326500120, 0.2394877259645100398 ) ) ;
#9559 = DIRECTION ( 'NONE',  ( 0.000000000000000000, 0.000000000000000000, -1.000000000000000000 ) ) ;
#9560 = DIRECTION ( 'NONE',  ( -0.5000000000000039968, 0.000000000000000000, -0.8660254037844362651 ) ) ;
#9561 = CARTESIAN_POINT ( 'NONE',  ( -1.964126537190517441, -2.749515453455440905, 0.1756903148397118697 ) ) ;
#9562 = ORIENTED_EDGE ( 'NONE', *, *, #5981, .F. ) ;
#9563 = CARTESIAN_POINT ( 'NONE',  ( -2.007201644623049841, -2.769458770238572676, 0.1575875454750225446 ) ) ;
#9564 = FACE_OUTER_BOUND ( 'NONE', #10510, .T. ) ;
#9565 = DIRECTION ( 'NONE',  ( 0.000000000000000000, 1.000000000000000000, 0.000000000000000000 ) ) ;
#9566 = ORIENTED_EDGE ( 'NONE', *, *, #1746, .F. ) ;
#9567 = ORIENTED_EDGE ( 'NONE', *, *, #11420, .F. ) ;
#9568 = CARTESIAN_POINT ( 'NONE',  ( -0.7114373258145173518, 1.190944881889763884, 0.3425575548946232507 ) ) ;
#9569 = DIRECTION ( 'NONE',  ( 0.000000000000000000, 0.000000000000000000, -1.000000000000000000 ) ) ;
#9570 = FACE_OUTER_BOUND ( 'NONE', #3066, .T. ) ;
#9571 = DIRECTION ( 'NONE',  ( -0.000000000000000000, -0.000000000000000000, 1.000000000000000000 ) ) ;
#9572 = DIRECTION ( 'NONE',  ( -1.000000000000000000, 0.000000000000000000, 0.000000000000000000 ) ) ;
#9573 = DIRECTION ( 'NONE',  ( -1.000000000000000000, 0.000000000000000000, 0.000000000000000000 ) ) ;
#9574 = EDGE_LOOP ( 'NONE', ( #6928, #14107, #11826, #9835 ) ) ;
#9575 = CARTESIAN_POINT ( 'NONE',  ( -1.607606113623940791, 0.09732815316530769867, -0.07192616626586137429 ) ) ;
#9576 = DIRECTION ( 'NONE',  ( 0.5000000000000004441, 8.673617379884095425E-15, -0.8660254037844384856 ) ) ;
#9577 = CARTESIAN_POINT ( 'NONE',  ( -0.7455328141524873997, 1.190944881889763884, 0.3622425942647021779 ) ) ;
#9578 = CARTESIAN_POINT ( 'NONE',  ( 8.678599364036360127E-17, 0.000000000000000000, 0.7086614173228346081 ) ) ;
#9579 = DIRECTION ( 'NONE',  ( 0.000000000000000000, -1.000000000000000000, 2.212657494868377674E-16 ) ) ;
#9580 = ORIENTED_EDGE ( 'NONE', *, *, #5506, .F. ) ;
#9581 = VERTEX_POINT ( 'NONE', #15388 ) ;
#9582 = ORIENTED_EDGE ( 'NONE', *, *, #12614, .F. ) ;
#9583 = ORIENTED_EDGE ( 'NONE', *, *, #5549, .F. ) ;
#9584 = EDGE_CURVE ( 'NONE', #12009, #12255, #2228, .T. ) ;
#9585 = DIRECTION ( 'NONE',  ( -1.000000000000000000, -0.000000000000000000, -0.000000000000000000 ) ) ;
#9586 = AXIS2_PLACEMENT_3D ( 'NONE', #10747, #26, #9569 ) ;
#9587 = TOROIDAL_SURFACE ( 'NONE', #14078, 0.04330708661417329020, 0.003937007874015747977 ) ;
#9588 = EDGE_CURVE ( 'NONE', #4902, #8242, #1182, .T. ) ;
#9589 = CIRCLE ( 'NONE', #11585, 0.01968503937007868437 ) ;
#9590 = SPHERICAL_SURFACE ( 'NONE', #4593, 0.01968503937007873988 ) ;
#9591 = LINE ( 'NONE', #45, #12345 ) ;
#9592 = CIRCLE ( 'NONE', #13086, 0.003937007874015741038 ) ;
#9593 = DIRECTION ( 'NONE',  ( 0.5000000000000054401, -8.326672684688674053E-17, 0.8660254037844354880 ) ) ;
#9594 = CARTESIAN_POINT ( 'NONE',  ( -0.2642136714276788201, -0.4881889763779528324, 0.03889220652917903254 ) ) ;
#9595 = DIRECTION ( 'NONE',  ( 0.4999999999999979461, 0.000000000000000000, 0.8660254037844398178 ) ) ;
#9596 = CARTESIAN_POINT ( 'NONE',  ( 0.000000000000000000, -0.09842519685039370636, 0.000000000000000000 ) ) ;
#9597 = EDGE_CURVE ( 'NONE', #11994, #7766, #5157, .T. ) ;
#9598 = DIRECTION ( 'NONE',  ( 7.230275848357267942E-16, -5.150430092931769150E-16, -1.000000000000000000 ) ) ;
#9599 = DIRECTION ( 'NONE',  ( 0.5000000000000172085, 0.000000000000000000, -0.8660254037844286046 ) ) ;
#9600 = CARTESIAN_POINT ( 'NONE',  ( 0.000000000000000000, 1.653543307086614567, -0.7007874015748031260 ) ) ;
#9601 = CYLINDRICAL_SURFACE ( 'NONE', #12672, 0.003937007874015740171 ) ;
#9602 = CIRCLE ( 'NONE', #6578, 0.003937007874015749712 ) ;
#9603 = AXIS2_PLACEMENT_3D ( 'NONE', #8673, #5207, #5444 ) ;
#9604 = ORIENTED_EDGE ( 'NONE', *, *, #12386, .F. ) ;
#9605 = CIRCLE ( 'NONE', #12853, 0.003937007874015758385 ) ;
#9606 = VERTEX_POINT ( 'NONE', #3548 ) ;
#9607 = TOROIDAL_SURFACE ( 'NONE', #6583, 0.7007874015748031260, 0.007874015748031495954 ) ;
#9608 = EDGE_LOOP ( 'NONE', ( #2770, #13295, #3435, #14059 ) ) ;
#9609 = ORIENTED_EDGE ( 'NONE', *, *, #79, .T. ) ;
#9610 = EDGE_CURVE ( 'NONE', #3678, #12240, #688, .T. ) ;
#9611 = EDGE_CURVE ( 'NONE', #4717, #15072, #431, .T. ) ;
#9612 = DIRECTION ( 'NONE',  ( 0.000000000000000000, 0.000000000000000000, -1.000000000000000000 ) ) ;
#9613 = MANIFOLD_SOLID_BREP ( 'Boss-Extrude2', #6607 ) ;
#9614 = DIRECTION ( 'NONE',  ( 0.9995479251422038081, -0.03006568382583900759, 0.000000000000000000 ) ) ;
#9615 = CIRCLE ( 'NONE', #11610, 0.7086614173228346081 ) ;
#9616 = AXIS2_PLACEMENT_3D ( 'NONE', #5668, #7869, #2163 ) ;
#9617 = CARTESIAN_POINT ( 'NONE',  ( 0.06692913385832209572, -0.4881889763779528324, -0.2377126739437405434 ) ) ;
#9618 = MECHANICAL_DESIGN_GEOMETRIC_PRESENTATION_REPRESENTATION (  '', ( #1360 ), #5590 ) ;
#9619 = EDGE_CURVE ( 'NONE', #7799, #115, #4422, .T. ) ;
#9620 = DIRECTION ( 'NONE',  ( -0.4999999999999981681, 0.000000000000000000, -0.8660254037844397068 ) ) ;
#9621 = CIRCLE ( 'NONE', #14873, 0.003937007874015741038 ) ;
#9622 = EDGE_CURVE ( 'NONE', #3832, #15072, #3175, .T. ) ;
#9623 = CIRCLE ( 'NONE', #10626, 0.01968503937007875723 ) ;
#9624 = FACE_OUTER_BOUND ( 'NONE', #12679, .T. ) ;
#9625 = ORIENTED_EDGE ( 'NONE', *, *, #991, .T. ) ;
#9626 = AXIS2_PLACEMENT_3D ( 'NONE', #8335, #3868, #12189 ) ;
#9627 = DIRECTION ( 'NONE',  ( -0.000000000000000000, -1.000000000000000000, -0.000000000000000000 ) ) ;
#9628 = CARTESIAN_POINT ( 'NONE',  ( -2.183651372152203507, -1.661851685721183136, -0.08366141732283423338 ) ) ;
#9629 = FACE_OUTER_BOUND ( 'NONE', #10972, .T. ) ;
#9630 = ORIENTED_EDGE ( 'NONE', *, *, #5038, .F. ) ;
#9631 = VERTEX_POINT ( 'NONE', #6260 ) ;
#9632 = AXIS2_PLACEMENT_3D ( 'NONE', #3242, #8084, #3164 ) ;
#9633 = AXIS2_PLACEMENT_3D ( 'NONE', #1458, #9599, #12266 ) ;
#9634 = AXIS2_PLACEMENT_3D ( 'NONE', #4612, #5704, #4293 ) ;
#9635 = AXIS2_PLACEMENT_3D ( 'NONE', #9888, #7519, #2811 ) ;
#9636 = ORIENTED_EDGE ( 'NONE', *, *, #5467, .T. ) ;
#9637 = AXIS2_PLACEMENT_3D ( 'NONE', #13254, #5010, #3928 ) ;
#9638 = EDGE_CURVE ( 'NONE', #2526, #9061, #4875, .T. ) ;
#9639 = CARTESIAN_POINT ( 'NONE',  ( -2.054789683517502574, -2.568945684013812070, 0.1522427580697409966 ) ) ;
#9640 = CARTESIAN_POINT ( 'NONE',  ( -1.579560462702055190, 0.1027931347612739549, 0.07190453453444432819 ) ) ;
#9641 = DIRECTION ( 'NONE',  ( 1.000000000000000000, -1.734723475976817507E-14, -3.009265538105091894E-28 ) ) ;
#9642 = EDGE_CURVE ( 'NONE', #15219, #6857, #11944, .T. ) ;
#9643 = CARTESIAN_POINT ( 'NONE',  ( -0.5405850968742077489, 1.037100910086446559, 0.2377418676363894090 ) ) ;
#9644 = EDGE_CURVE ( 'NONE', #10586, #8739, #1217, .T. ) ;
#9645 = CARTESIAN_POINT ( 'NONE',  ( 0.1062992125984796865, -0.1023622047244094474, -0.5870514566507987197 ) ) ;
#9646 = VECTOR ( 'NONE', #2751, 39.37007874015748143 ) ;
#9647 = FACE_OUTER_BOUND ( 'NONE', #6039, .T. ) ;
#9648 = AXIS2_PLACEMENT_3D ( 'NONE', #10056, #6359, #10223 ) ;
#9649 = CARTESIAN_POINT ( 'NONE',  ( -1.943431940181322481, -2.816572830930641036, 0.1716618975443832407 ) ) ;
#9650 = CIRCLE ( 'NONE', #2873, 0.05298991407461853265 ) ;
#9651 = EDGE_LOOP ( 'NONE', ( #425, #6309, #10777, #7036 ) ) ;
#9652 = CARTESIAN_POINT ( 'NONE',  ( -1.980093622780896956, -2.844111206679635906, 0.1439326711935206005 ) ) ;
#9653 = AXIS2_PLACEMENT_3D ( 'NONE', #3271, #14009, #3513 ) ;
#9654 = CARTESIAN_POINT ( 'NONE',  ( -0.04509495097506254629, 0.1479884890110657880, -0.05203401519686126631 ) ) ;
#9655 = ORIENTED_EDGE ( 'NONE', *, *, #5974, .T. ) ;
#9656 = ADVANCED_FACE ( 'NONE', ( #10989 ), #13187, .F. ) ;
#9657 = ORIENTED_EDGE ( 'NONE', *, *, #13589, .T. ) ;
#9659 = ORIENTED_EDGE ( 'NONE', *, *, #14448, .F. ) ;
#9658 = CIRCLE ( 'NONE', #10882, 0.003937007874015724558 ) ;
#9660 = AXIS2_PLACEMENT_3D ( 'NONE', #4830, #12998, #2190 ) ;
#9661 = AXIS2_PLACEMENT_3D ( 'NONE', #882, #4554, #14042 ) ;
#9662 = CARTESIAN_POINT ( 'NONE',  ( 0.000000000000000000, 1.346456692913385877, 0.000000000000000000 ) ) ;
#9663 = VECTOR ( 'NONE', #5909, 39.37007874015748143 ) ;
#9664 = CARTESIAN_POINT ( 'NONE',  ( 0.000000000000000000, 0.000000000000000000, 0.000000000000000000 ) ) ;
#9665 = DIRECTION ( 'NONE',  ( 0.000000000000000000, 0.000000000000000000, 1.000000000000000000 ) ) ;
#9666 = DIRECTION ( 'NONE',  ( 1.000000000000000000, 0.000000000000000000, 1.224646799147353207E-16 ) ) ;
#9667 = DIRECTION ( 'NONE',  ( 0.000000000000000000, 0.000000000000000000, -1.000000000000000000 ) ) ;
#9668 = LINE ( 'NONE', #8482, #863 ) ;
#9669 = ORIENTED_EDGE ( 'NONE', *, *, #8287, .T. ) ;
#9670 = CARTESIAN_POINT ( 'NONE',  ( -1.599731447215878788, 0.1084887237743279165, -0.04822519498669181059 ) ) ;
#9671 = DIRECTION ( 'NONE',  ( 1.000000000000000000, 0.000000000000000000, 0.000000000000000000 ) ) ;
#9672 = AXIS2_PLACEMENT_3D ( 'NONE', #464, #13588, #9939 ) ;
#9673 = AXIS2_PLACEMENT_3D ( 'NONE', #10162, #11974, #1070 ) ;
#9674 = CARTESIAN_POINT ( 'NONE',  ( -0.06972667172716363881, -0.1870117487642863896, 0.03937007824553747509 ) ) ;
#9675 = ADVANCED_FACE ( 'NONE', ( #14452 ), #1353, .F. ) ;
#9676 = DIRECTION ( 'NONE',  ( 1.445602896647339903E-16, 0.000000000000000000, -1.000000000000000000 ) ) ;
#9677 = VECTOR ( 'NONE', #13892, 39.37007874015748143 ) ;
#9678 = VERTEX_POINT ( 'NONE', #335 ) ;
#9679 = ORIENTED_EDGE ( 'NONE', *, *, #7009, .F. ) ;
#9680 = ORIENTED_EDGE ( 'NONE', *, *, #3481, .T. ) ;
#9681 = ORIENTED_EDGE ( 'NONE', *, *, #7986, .T. ) ;
#9682 = CYLINDRICAL_SURFACE ( 'NONE', #10646, 0.1771653543307079026 ) ;
#9683 = VECTOR ( 'NONE', #7477, 39.37007874015748143 ) ;
#9684 = CARTESIAN_POINT ( 'NONE',  ( 0.000000000000000000, 2.165354330708661568, 0.000000000000000000 ) ) ;
#9685 = DIRECTION ( 'NONE',  ( -0.000000000000000000, -1.000000000000000000, -0.000000000000000000 ) ) ;
#9686 = DIRECTION ( 'NONE',  ( 0.1305055777265676509, 0.9885803249658943193, -0.07534743043118244388 ) ) ;
#9687 = DIRECTION ( 'NONE',  ( 0.4999999999999979461, 0.000000000000000000, 0.8660254037844398178 ) ) ;
#9688 = CARTESIAN_POINT ( 'NONE',  ( -0.07545607570875816072, 0.1645859079935992897, 0.03937007874015746589 ) ) ;
#9689 = DIRECTION ( 'NONE',  ( -0.000000000000000000, -1.000000000000000000, -0.000000000000000000 ) ) ;
#9690 = CIRCLE ( 'NONE', #12444, 0.003937007874015749712 ) ;
#9691 = FACE_OUTER_BOUND ( 'NONE', #7134, .T. ) ;
#9692 = CARTESIAN_POINT ( 'NONE',  ( -1.580259682937577903, 0.1018956540318208953, -0.04477369844328074611 ) ) ;
#9693 = CARTESIAN_POINT ( 'NONE',  ( 0.5905511811023622659, -0.2952755905511811330, -0.4584677793364514420 ) ) ;
#9694 = AXIS2_PLACEMENT_3D ( 'NONE', #652, #12400, #1670 ) ;
#9695 = EDGE_CURVE ( 'NONE', #11304, #161, #7177, .T. ) ;
#9696 = ORIENTED_EDGE ( 'NONE', *, *, #151, .T. ) ;
#9697 = ORIENTED_EDGE ( 'NONE', *, *, #7416, .F. ) ;
#9698 = TOROIDAL_SURFACE ( 'NONE', #13192, 2.194881889763779181, 0.01968503937007873988 ) ;
#9699 = ORIENTED_EDGE ( 'NONE', *, *, #13311, .T. ) ;
#9700 = ADVANCED_FACE ( 'NONE', ( #14682 ), #11690, .T. ) ;
#9701 = CARTESIAN_POINT ( 'NONE',  ( 7.232166136696967594E-17, 0.5984251968503937480, 0.5905511811023621549 ) ) ;
#9702 = DIRECTION ( 'NONE',  ( -1.000000000000000000, -0.000000000000000000, -3.075191616504340279E-15 ) ) ;
#9703 = VECTOR ( 'NONE', #7411, 39.37007874015748143 ) ;
#9704 = CARTESIAN_POINT ( 'NONE',  ( 0.03346456692910666081, -0.4881889763779528324, -0.05796233017450189845 ) ) ;
#9705 = CARTESIAN_POINT ( 'NONE',  ( 0.2373612774290684013, -0.4921259842519685179, 0.06430355563125962626 ) ) ;
#9706 = DIRECTION ( 'NONE',  ( -0.5000000000000035527, -0.000000000000000000, 0.8660254037844365982 ) ) ;
#9707 = AXIS2_PLACEMENT_3D ( 'NONE', #5730, #3547, #1052 ) ;
#9708 = FACE_OUTER_BOUND ( 'NONE', #1409, .T. ) ;
#9709 = DIRECTION ( 'NONE',  ( 0.000000000000000000, -1.000000000000000000, 0.000000000000000000 ) ) ;
#9710 = CARTESIAN_POINT ( 'NONE',  ( 0.1023622047244638067, -0.1023622047244094474, -0.2472069366676780122 ) ) ;
#9711 = DIRECTION ( 'NONE',  ( 0.000000000000000000, 0.000000000000000000, -1.000000000000000000 ) ) ;
#9712 = EDGE_CURVE ( 'NONE', #10775, #1163, #14522, .T. ) ;
#9713 = ADVANCED_FACE ( 'NONE', ( #37 ), #269, .F. ) ;
#9714 = VERTEX_POINT ( 'NONE', #3635 ) ;
#9715 = ORIENTED_EDGE ( 'NONE', *, *, #8663, .F. ) ;
#9716 = VECTOR ( 'NONE', #1700, 39.37007874015748143 ) ;
#9717 = B_SPLINE_CURVE_WITH_KNOTS ( 'NONE', 3,
 ( #12023, #14358, #6033, #3937, #6195, #9817, #6259, #8635, #13263, #13327 ),
 .UNSPECIFIED., .F., .F.,
 ( 4, 2, 2, 2, 4 ),
 ( 0.000000000000000000, 0.0006575499428678712377, 0.001315099885735742475, 0.001972649828603614038, 0.002630199771471484517 ),
 .UNSPECIFIED. ) ;
#9718 = APPLICATION_CONTEXT ( 'automotive_design' ) ;
#9719 = ADVANCED_FACE ( 'NONE', ( #8413 ), #7838, .F. ) ;
#9720 = VERTEX_POINT ( 'NONE', #5319 ) ;
#9721 = AXIS2_PLACEMENT_3D ( 'NONE', #13079, #10890, #10739 ) ;
#9722 = CARTESIAN_POINT ( 'NONE',  ( 1.181102362204724310, 4.044111181948214319E-16, 0.02559055118110236185 ) ) ;
#9723 = CARTESIAN_POINT ( 'NONE',  ( 0.000000000000000000, 0.05905511811023622659, 0.000000000000000000 ) ) ;
#9724 = CARTESIAN_POINT ( 'NONE',  ( 0.000000000000000000, 0.5984251968503937480, 0.000000000000000000 ) ) ;
#9725 = DIRECTION ( 'NONE',  ( -0.000000000000000000, 1.000000000000000000, 0.000000000000000000 ) ) ;
#9727 = AXIS2_PLACEMENT_3D ( 'NONE', #11449, #5542, #7992 ) ;
#9726 = CARTESIAN_POINT ( 'NONE',  ( 0.000000000000000000, 0.000000000000000000, 0.08858267716535432601 ) ) ;
#9728 = CARTESIAN_POINT ( 'NONE',  ( -1.979213154580101275, -2.704552134622930204, 0.1698516854049418046 ) ) ;
#9729 = ORIENTED_EDGE ( 'NONE', *, *, #4801, .F. ) ;
#9730 = CARTESIAN_POINT ( 'NONE',  ( -1.959343309635757757, -2.897611896471060433, 0.1048995451756935399 ) ) ;
#9731 = ADVANCED_FACE ( 'NONE', ( #4082 ), #15053, .F. ) ;
#9732 = CARTESIAN_POINT ( 'NONE',  ( -0.3294846884549020305, -0.2952755905511811330, 0.2675111804726948983 ) ) ;
#9733 = TOROIDAL_SURFACE ( 'NONE', #4211, 0.007874015748031495954, 0.003937007874015747977 ) ;
#9734 = FACE_OUTER_BOUND ( 'NONE', #10372, .T. ) ;
#9735 = ADVANCED_FACE ( 'NONE', ( #10274, #9978 ), #14991, .F. ) ;
#9736 = EDGE_LOOP ( 'NONE', ( #11320, #9965, #5155, #2519 ) ) ;
#9737 = EDGE_LOOP ( 'NONE', ( #7198, #15133, #14488 ) ) ;
#9738 = ADVANCED_FACE ( 'NONE', ( #4014 ), #4167, .T. ) ;
#9739 = ORIENTED_EDGE ( 'NONE', *, *, #5801, .F. ) ;
#9740 = CYLINDRICAL_SURFACE ( 'NONE', #5862, 0.01968503937007875723 ) ;
#9741 = DIRECTION ( 'NONE',  ( 0.8660254037844365982, -0.000000000000000000, 0.5000000000000035527 ) ) ;
#9742 = ADVANCED_FACE ( 'NONE', ( #8789 ), #7604, .T. ) ;
#9743 = DIRECTION ( 'NONE',  ( -0.000000000000000000, -0.000000000000000000, -1.000000000000000000 ) ) ;
#9744 = CARTESIAN_POINT ( 'NONE',  ( 0.09842519685044820443, -0.4881889763779528324, -0.5870514566507987197 ) ) ;
#9745 = ITEM_DEFINED_TRANSFORMATION ( 'NONE', 'NONE', #4363,  #11481 ) ;
#9746 = DIRECTION ( 'NONE',  ( 0.000000000000000000, -1.000000000000000000, 1.734723475976817507E-14 ) ) ;
#9747 = CARTESIAN_POINT ( 'NONE',  ( -0.05905511811023622659, 1.338626482899105241, -0.5946706712680680518 ) ) ;
#9748 = ORIENTED_EDGE ( 'NONE', *, *, #12282, .F. ) ;
#9749 = CARTESIAN_POINT ( 'NONE',  ( -1.596214514379631577, 0.1135332894430610556, -0.07535569387266634334 ) ) ;
#9750 = CARTESIAN_POINT ( 'NONE',  ( 0.1743691514447621993, -0.1023622047244094474, 0.1734091183126679481 ) ) ;
#9751 = CARTESIAN_POINT ( 'NONE',  ( -0.03452177266044149928, -0.1823242888858135624, 0.02287309002717315826 ) ) ;
#9752 = DIRECTION ( 'NONE',  ( 0.000000000000000000, 4.956352788505160310E-16, 1.000000000000000000 ) ) ;
#9753 = VERTEX_POINT ( 'NONE', #10126 ) ;
#9754 = MANIFOLD_SOLID_BREP ( 'Fillet5', #12378 ) ;
#9755 = VERTEX_POINT ( 'NONE', #13800 ) ;
#9756 = EDGE_CURVE ( 'NONE', #5246, #9837, #10929, .T. ) ;
#9757 = ORIENTED_EDGE ( 'NONE', *, *, #8488, .F. ) ;
#9758 = ORIENTED_EDGE ( 'NONE', *, *, #7579, .T. ) ;
#9759 = DIRECTION ( 'NONE',  ( 0.5000000000000008882, -0.000000000000000000, -0.8660254037844380415 ) ) ;
#9760 = ADVANCED_FACE ( 'NONE', ( #2995 ), #11459, .T. ) ;
#9761 = EDGE_CURVE ( 'NONE', #3987, #253, #12937, .T. ) ;
#9762 = DIRECTION ( 'NONE',  ( 0.000000000000000000, 0.000000000000000000, -1.000000000000000000 ) ) ;
#9763 = LINE ( 'NONE', #3725, #7833 ) ;
#9764 = DIRECTION ( 'NONE',  ( 0.5000000000000054401, -8.326672683921270165E-17, 0.8660254037844354880 ) ) ;
#9765 =( NAMED_UNIT ( * ) PLANE_ANGLE_UNIT ( ) SI_UNIT ( $, .RADIAN. ) );
#9766 = DIRECTION ( 'NONE',  ( 0.000000000000000000, 0.000000000000000000, -1.000000000000000000 ) ) ;
#9767 = LINE ( 'NONE', #5032, #4388 ) ;
#9768 = DIRECTION ( 'NONE',  ( 0.000000000000000000, 0.000000000000000000, 1.000000000000000000 ) ) ;
#9769 = DIRECTION ( 'NONE',  ( 1.224646799147353207E-16, 1.000000000000000000, -0.000000000000000000 ) ) ;
#9770 = ORIENTED_EDGE ( 'NONE', *, *, #13651, .F. ) ;
#9771 = ORIENTED_EDGE ( 'NONE', *, *, #1986, .T. ) ;
#9772 = ORIENTED_EDGE ( 'NONE', *, *, #7009, .T. ) ;
#9773 = PRODUCT_DEFINITION ( 'UNKNOWN', '', #15384, #6723 ) ;
#9774 = CARTESIAN_POINT ( 'NONE',  ( 0.4822834645669299980, -0.1023622047244094474, 0.3466374647693608591 ) ) ;
#9775 = CARTESIAN_POINT ( 'NONE',  ( 8.196454954923229282E-17, 1.606299212598425674, 0.6692913385826770867 ) ) ;
#9776 = DIRECTION ( 'NONE',  ( 1.000000000000000000, 0.000000000000000000, 0.000000000000000000 ) ) ;
#9777 = DIRECTION ( 'NONE',  ( 1.000000000000000000, 0.000000000000000000, -0.000000000000000000 ) ) ;
#9778 = CARTESIAN_POINT ( 'NONE',  ( 0.000000000000000000, 0.000000000000000000, -0.7086614173228346081 ) ) ;
#9779 = SPHERICAL_SURFACE ( 'NONE', #5140, 0.003937007874015747977 ) ;
#9780 = LINE ( 'NONE', #3672, #11841 ) ;
#9781 = DIRECTION ( 'NONE',  ( -0.8660254037844433705, 0.000000000000000000, -0.4999999999999918954 ) ) ;
#9782 = ORIENTED_EDGE ( 'NONE', *, *, #5942, .T. ) ;
#9783 = ORIENTED_EDGE ( 'NONE', *, *, #11703, .F. ) ;
#9784 = ORIENTED_EDGE ( 'NONE', *, *, #1868, .T. ) ;
#9785 = VERTEX_POINT ( 'NONE', #11372 ) ;
#9786 = VERTEX_POINT ( 'NONE', #1579 ) ;
#9787 = CYLINDRICAL_SURFACE ( 'NONE', #13627, 0.03937007874015751446 ) ;
#9788 = ADVANCED_FACE ( 'NONE', ( #5410 ), #9184, .F. ) ;
#9789 = EDGE_CURVE ( 'NONE', #9720, #4762, #6657, .T. ) ;
#9790 = CARTESIAN_POINT ( 'NONE',  ( 0.5445274672588121812, 1.338626482899105241, 0.2461921031270739857 ) ) ;
#9791 = DIRECTION ( 'NONE',  ( 1.000000000000000000, 0.000000000000000000, 0.000000000000000000 ) ) ;
#9792 = LINE ( 'NONE', #14497, #6825 ) ;
#9793 = DIRECTION ( 'NONE',  ( -0.000000000000000000, -1.000000000000000000, -0.000000000000000000 ) ) ;
#9794 = CARTESIAN_POINT ( 'NONE',  ( -1.888395665188653094, -2.901081385897817277, -0.1225630396599474148 ) ) ;
#9795 = ORIENTED_EDGE ( 'NONE', *, *, #4793, .T. ) ;
#9796 = CARTESIAN_POINT ( 'NONE',  ( -1.943333224563443595, -2.937028733817375947, 0.01142278406163464016 ) ) ;
#9797 = EDGE_CURVE ( 'NONE', #9010, #8101, #12941, .T. ) ;
#9798 = CARTESIAN_POINT ( 'NONE',  ( -0.5068643957866975081, 1.043307086614173373, 0.2244473186741497150 ) ) ;
#9799 = ORIENTED_EDGE ( 'NONE', *, *, #4659, .T. ) ;
#9800 = ORIENTED_EDGE ( 'NONE', *, *, #14792, .F. ) ;
#9801 = PRODUCT ( 'MAT-022', 'MAT-022', '', ( #663 ) ) ;
#9802 = EDGE_LOOP ( 'NONE', ( #8630, #13258, #8862, #9031 ) ) ;
#9803 = FACE_OUTER_BOUND ( 'NONE', #7561, .T. ) ;
#9804 = ADVANCED_FACE ( 'NONE', ( #2040 ), #10694, .T. ) ;
#9805 = DIRECTION ( 'NONE',  ( 0.000000000000000000, 1.000000000000000000, 0.000000000000000000 ) ) ;
#9806 = EDGE_CURVE ( 'NONE', #2439, #9943, #9191, .T. ) ;
#9807 = AXIS2_PLACEMENT_3D ( 'NONE', #2154, #6831, #12740 ) ;
#9808 = DIRECTION ( 'NONE',  ( -8.881784197001253901E-15, 0.000000000000000000, -1.000000000000000000 ) ) ;
#9809 = DIRECTION ( 'NONE',  ( -1.301042606982607687E-14, 0.000000000000000000, 1.000000000000000000 ) ) ;
#9810 = DIRECTION ( 'NONE',  ( -1.224646799147352961E-16, 0.000000000000000000, -1.000000000000000000 ) ) ;
#9811 = DIRECTION ( 'NONE',  ( 1.224646799147353700E-16, 0.000000000000000000, -1.000000000000000000 ) ) ;
#9812 = VERTEX_POINT ( 'NONE', #15132 ) ;
#9813 = DIRECTION ( 'NONE',  ( -0.5000000000000001110, 0.000000000000000000, -0.8660254037844385966 ) ) ;
#9814 = ADVANCED_FACE ( 'NONE', ( #4478 ), #9259, .F. ) ;
#9815 = CARTESIAN_POINT ( 'NONE',  ( -1.591501945092674841, 0.08600752902535276079, -0.08366141732283462196 ) ) ;
#9816 = DIRECTION ( 'NONE',  ( 0.5000000000000035527, -0.000000000000000000, -0.8660254037844365982 ) ) ;
#9817 = CARTESIAN_POINT ( 'NONE',  ( -0.02371960882139430987, -0.1628608293428424891, 0.03730919803856837247 ) ) ;
#9818 = DIRECTION ( 'NONE',  ( 0.000000000000000000, 1.000000000000000000, 0.000000000000000000 ) ) ;
#9819 = ORIENTED_EDGE ( 'NONE', *, *, #308, .F. ) ;
#9820 = VERTEX_POINT ( 'NONE', #11528 ) ;
#9821 = ORIENTED_EDGE ( 'NONE', *, *, #3314, .F. ) ;
#9822 = FACE_OUTER_BOUND ( 'NONE', #11038, .T. ) ;
#9823 = CARTESIAN_POINT ( 'NONE',  ( 0.1724006475077543565, -0.09842519685039370636, 0.1689446513984334541 ) ) ;
#9824 = CARTESIAN_POINT ( 'NONE',  ( -2.061751060645342637, -2.382911221804981494, 0.1354770691259033766 ) ) ;
#9825 = CARTESIAN_POINT ( 'NONE',  ( 0.1181102362204452250, 35.08612325493803041, -1.395267672073842613 ) ) ;
#9826 = DIRECTION ( 'NONE',  ( -0.8660254037844385966, -0.000000000000000000, 0.4999999999999998890 ) ) ;
#9827 = LINE ( 'NONE', #1230, #11357 ) ;
#9828 = CARTESIAN_POINT ( 'NONE',  ( 0.4462573421471743851, -0.2952755905511811330, 0.1439951688233476745 ) ) ;
#9829 = FACE_OUTER_BOUND ( 'NONE', #7463, .T. ) ;
#9830 = EDGE_CURVE ( 'NONE', #13377, #241, #13700, .T. ) ;
#9831 = FACE_OUTER_BOUND ( 'NONE', #1404, .T. ) ;
#9832 = CARTESIAN_POINT ( 'NONE',  ( 0.5595825771504284729, -0.4881889763779528324, 0.2048774586467246028 ) ) ;
#9833 = ORIENTED_EDGE ( 'NONE', *, *, #8280, .T. ) ;
#9834 = ADVANCED_FACE ( 'NONE', ( #3383 ), #793, .T. ) ;
#9835 = ORIENTED_EDGE ( 'NONE', *, *, #8555, .T. ) ;
#9836 = TOROIDAL_SURFACE ( 'NONE', #10073, 0.5984251968503937480, 0.007874015748031495954 ) ;
#9837 = VERTEX_POINT ( 'NONE', #3299 ) ;
#9838 = CIRCLE ( 'NONE', #4320, 0.003937007874015750579 ) ;
#9839 = AXIS2_PLACEMENT_3D ( 'NONE', #4807, #8270, #129 ) ;
#9840 = DIRECTION ( 'NONE',  ( 0.8660254037844383745, 0.000000000000000000, -0.5000000000000004441 ) ) ;
#9841 = CARTESIAN_POINT ( 'NONE',  ( -1.945283543323844455, -2.932305031303924281, 0.03979015993530637257 ) ) ;
#9842 = DIRECTION ( 'NONE',  ( 1.000000000000000000, 0.000000000000000000, 0.000000000000000000 ) ) ;
#9843 = CARTESIAN_POINT ( 'NONE',  ( -1.181102362204724310, 0.000000000000000000, 0.02559055118110236185 ) ) ;
#9844 = CARTESIAN_POINT ( 'NONE',  ( -1.574484809660005480, 0.1100025355994808662, -0.06175692796176408816 ) ) ;
#9845 = DIRECTION ( 'NONE',  ( 1.000000000000000000, 0.000000000000000000, 0.000000000000000000 ) ) ;
#9846 = AXIS2_PLACEMENT_3D ( 'NONE', #11328, #9741, #4051 ) ;
#9847 = AXIS2_PLACEMENT_3D ( 'NONE', #1703, #8910, #13917 ) ;
#9848 = FACE_OUTER_BOUND ( 'NONE', #5490, .T. ) ;
#9849 = DIRECTION ( 'NONE',  ( -1.224646799147353947E-16, 0.000000000000000000, -1.000000000000000000 ) ) ;
#9850 = DIRECTION ( 'NONE',  ( -0.8011800915434517112, 0.5984233124757307731, 0.000000000000000000 ) ) ;
#9851 = DIRECTION ( 'NONE',  ( 0.000000000000000000, 1.000000000000000000, 0.000000000000000000 ) ) ;
#9852 = CIRCLE ( 'NONE', #10345, 0.01968503937007873988 ) ;
#9853 = ORIENTED_EDGE ( 'NONE', *, *, #1012, .T. ) ;
#9854 = EDGE_CURVE ( 'NONE', #6744, #9415, #8206, .T. ) ;
#9855 = EDGE_LOOP ( 'NONE', ( #13312, #14288, #1181, #7964 ) ) ;
#9856 = EDGE_LOOP ( 'NONE', ( #4752, #13104 ) ) ;
#9857 = VERTEX_POINT ( 'NONE', #12854 ) ;
#9858 = ORIENTED_EDGE ( 'NONE', *, *, #11604, .F. ) ;
#9859 = AXIS2_PLACEMENT_3D ( 'NONE', #12431, #6458, #10064 ) ;
#9860 = AXIS2_PLACEMENT_3D ( 'NONE', #12098, #44, #1149 ) ;
#9861 = CARTESIAN_POINT ( 'NONE',  ( -1.403185310738388036, -0.03069143131531506044, -0.04402505006082085837 ) ) ;
#9862 = VECTOR ( 'NONE', #5607, 39.37007874015749564 ) ;
#9863 = VECTOR ( 'NONE', #4602, 39.37007874015748854 ) ;
#9864 = DIRECTION ( 'NONE',  ( 0.000000000000000000, 0.000000000000000000, 1.000000000000000000 ) ) ;
#9865 = AXIS2_PLACEMENT_3D ( 'NONE', #885, #9571, #974 ) ;
#9866 = CARTESIAN_POINT ( 'NONE',  ( -0.1028896637645180384, -0.1023622047244094474, -0.2462933508112025438 ) ) ;
#9867 = CARTESIAN_POINT ( 'NONE',  ( -1.141732283464566677, 4.821444091131319228E-18, 0.02952755905511811330 ) ) ;
#9868 = DIRECTION ( 'NONE',  ( 0.000000000000000000, 0.000000000000000000, 1.000000000000000000 ) ) ;
#9869 = CYLINDRICAL_SURFACE ( 'NONE', #7219, 0.003937007874015749712 ) ;
#9870 = CARTESIAN_POINT ( 'NONE',  ( -1.879680948933423856, -2.922298401170338344, 0.01183035193844450030 ) ) ;
#9871 = ORIENTED_EDGE ( 'NONE', *, *, #923, .T. ) ;
#9872 = DIRECTION ( 'NONE',  ( 0.000000000000000000, 1.000000000000000000, 0.000000000000000000 ) ) ;
#9873 = DIRECTION ( 'NONE',  ( -0.000000000000000000, -0.000000000000000000, -1.000000000000000000 ) ) ;
#9874 = CIRCLE ( 'NONE', #12374, 0.5905511811023621549 ) ;
#9875 = AXIS2_PLACEMENT_3D ( 'NONE', #8567, #10926, #9768 ) ;
#9876 = DIRECTION ( 'NONE',  ( 1.000000000000000000, 0.000000000000000000, 0.000000000000000000 ) ) ;
#9877 = VERTEX_POINT ( 'NONE', #15368 ) ;
#9878 = AXIS2_PLACEMENT_3D ( 'NONE', #7825, #11447, #2111 ) ;
#9879 = ORIENTED_EDGE ( 'NONE', *, *, #11500, .F. ) ;
#9880 = AXIS2_PLACEMENT_3D ( 'NONE', #14923, #3161, #6748 ) ;
#9881 = ADVANCED_FACE ( 'NONE', ( #4547 ), #9329, .T. ) ;
#9882 = AXIS2_PLACEMENT_3D ( 'NONE', #7535, #1913, #3952 ) ;
#9883 = ORIENTED_EDGE ( 'NONE', *, *, #5250, .T. ) ;
#9884 = B_SPLINE_CURVE_WITH_KNOTS ( 'NONE', 3,
 ( #10927, #218, #13125, #14304, #5988, #7601, #3564, #6139, #12481, #8569 ),
 .UNSPECIFIED., .F., .F.,
 ( 4, 2, 2, 2, 4 ),
 ( 0.000000000000000000, 0.0003853806145889340524, 0.0007707612291778681048, 0.001156141843766802157, 0.001541522458355736210 ),
 .UNSPECIFIED. ) ;
#9885 = ADVANCED_FACE ( 'NONE', ( #6984 ), #6941, .T. ) ;
#9886 = VECTOR ( 'NONE', #4559, 39.37007874015748143 ) ;
#9887 = VECTOR ( 'NONE', #10289, 39.37007874015748143 ) ;
#9888 = CARTESIAN_POINT ( 'NONE',  ( -0.2362204724409448231, -0.02638708502139245488, -0.03937007874015747977 ) ) ;
#9889 = DIRECTION ( 'NONE',  ( 0.8144815189573203495, -0.5801894994542524664, 0.000000000000000000 ) ) ;
#9890 = DIRECTION ( 'NONE',  ( 0.000000000000000000, 0.000000000000000000, -1.000000000000000000 ) ) ;
#9891 = AXIS2_PLACEMENT_3D ( 'NONE', #13317, #13409, #6106 ) ;
#9892 = CARTESIAN_POINT ( 'NONE',  ( -0.01656597074380673426, -0.1797544903306477204, -0.02941166498823429704 ) ) ;
#9893 = ORIENTED_EDGE ( 'NONE', *, *, #1087, .F. ) ;
#9894 = CARTESIAN_POINT ( 'NONE',  ( -0.2393297813659120143, -0.4921259842519685179, 0.06089400679736763772 ) ) ;
#9895 = CARTESIAN_POINT ( 'NONE',  ( -0.05114323250695503725, 0.05905511811023622659, -0.08858267716535432601 ) ) ;
#9896 = DIRECTION ( 'NONE',  ( 0.000000000000000000, -8.673617379884013384E-15, 1.000000000000000000 ) ) ;
#9897 = FACE_OUTER_BOUND ( 'NONE', #1134, .T. ) ;
#9898 = EDGE_CURVE ( 'NONE', #12256, #1879, #11185, .T. ) ;
#9899 = CIRCLE ( 'NONE', #5366, 0.03937007874015751446 ) ;
#9900 = AXIS2_PLACEMENT_3D ( 'NONE', #12252, #10908, #13325 ) ;
#9901 = EDGE_CURVE ( 'NONE', #9995, #10028, #5504, .T. ) ;
#9902 = CIRCLE ( 'NONE', #4373, 0.03937007874015751446 ) ;
#9903 = EDGE_LOOP ( 'NONE', ( #10802, #604, #10171, #4461 ) ) ;
#9904 = ORIENTED_EDGE ( 'NONE', *, *, #3103, .F. ) ;
#9905 = VERTEX_POINT ( 'NONE', #11501 ) ;
#9906 = ADVANCED_FACE ( 'NONE', ( #13611 ), #10174, .F. ) ;
#9907 = LINE ( 'NONE', #274, #8409 ) ;
#9908 = PLANE ( 'NONE',  #11910 ) ;
#9909 = DIRECTION ( 'NONE',  ( -0.5000000000000001110, -0.000000000000000000, 0.8660254037844385966 ) ) ;
#9910 = DIRECTION ( 'NONE',  ( 0.000000000000000000, 0.000000000000000000, 1.000000000000000000 ) ) ;
#9911 = APPLICATION_PROTOCOL_DEFINITION ( 'draft international standard', 'automotive_design', 1998, #3510 ) ;
#9912 = AXIS2_PLACEMENT_3D ( 'NONE', #9057, #13827, #3101 ) ;
#9913 = CARTESIAN_POINT ( 'NONE',  ( 0.05175539059627461136, 0.07874015748031495954, -0.07475334604056278753 ) ) ;
#9914 = CIRCLE ( 'NONE', #654, 0.6692913385826770867 ) ;
#9915 = CARTESIAN_POINT ( 'NONE',  ( -1.985311755390326782, -2.772329397582949717, -0.1771653543307079026 ) ) ;
#9916 = AXIS2_PLACEMENT_3D ( 'NONE', #9984, #14762, #504 ) ;
#9917 = CARTESIAN_POINT ( 'NONE',  ( -0.06604848736013260724, 1.035433070866141891, -0.5868460571724354313 ) ) ;
#9918 = CARTESIAN_POINT ( 'NONE',  ( 0.000000000000000000, 0.4094488188976377896, 0.000000000000000000 ) ) ;
#9919 = AXIS2_PLACEMENT_3D ( 'NONE', #9369, #15248, #14300 ) ;
#9920 =( REPRESENTATION_RELATIONSHIP ('NONE','NONE', #8904, #2403 ) REPRESENTATION_RELATIONSHIP_WITH_TRANSFORMATION ( #12953 )SHAPE_REPRESENTATION_RELATIONSHIP( ) );
#9921 = DIRECTION ( 'NONE',  ( 0.000000000000000000, 0.000000000000000000, -1.000000000000000000 ) ) ;
#9922 = ORIENTED_EDGE ( 'NONE', *, *, #7603, .T. ) ;
#9923 = ADVANCED_FACE ( 'NONE', ( #6479 ), #698, .T. ) ;
#9924 = ORIENTED_EDGE ( 'NONE', *, *, #8374, .T. ) ;
#9925 = DIRECTION ( 'NONE',  ( 0.000000000000000000, 0.000000000000000000, 1.000000000000000000 ) ) ;
#9926 = ORIENTED_EDGE ( 'NONE', *, *, #3154, .T. ) ;
#9927 = AXIS2_PLACEMENT_3D ( 'NONE', #11238, #7628, #4101 ) ;
#9928 = EDGE_CURVE ( 'NONE', #7929, #2402, #4215, .T. ) ;
#9929 = ADVANCED_FACE ( 'NONE', ( #7894 ), #3203, .T. ) ;
#9930 = AXIS2_PLACEMENT_3D ( 'NONE', #11858, #9346, #979 ) ;
#9931 = CARTESIAN_POINT ( 'NONE',  ( -0.002500327830563101039, -0.1605493263772690415, 0.000000000000000000 ) ) ;
#9932 = CARTESIAN_POINT ( 'NONE',  ( -1.939282332474665305, -2.946842880316514979, 0.03118749810191574420 ) ) ;
#9933 = DIRECTION ( 'NONE',  ( 0.4999999999999979461, 0.000000000000000000, 0.8660254037844398178 ) ) ;
#9934 = CARTESIAN_POINT ( 'NONE',  ( -1.580259682937507515, 0.1018956540318726595, -0.04477369844321319597 ) ) ;
#9935 = EDGE_CURVE ( 'NONE', #5321, #14143, #14957, .T. ) ;
#9936 = DIRECTION ( 'NONE',  ( -0.000000000000000000, -1.000000000000000000, -0.000000000000000000 ) ) ;
#9937 = CARTESIAN_POINT ( 'NONE',  ( -1.509677571405407148, 0.2301488344313167012, 0.03937007874015747977 ) ) ;
#9938 = AXIS2_PLACEMENT_3D ( 'NONE', #11864, #1137, #4732 ) ;
#9939 = DIRECTION ( 'NONE',  ( -4.336808689942014285E-16, 0.000000000000000000, 1.000000000000000000 ) ) ;
#9940 = CARTESIAN_POINT ( 'NONE',  ( -1.880307312777807827, -2.920775457401061814, -0.02280129370432555300 ) ) ;
#9941 = DIRECTION ( 'NONE',  ( 0.000000000000000000, 1.000000000000000000, 0.000000000000000000 ) ) ;
#9942 = VECTOR ( 'NONE', #5086, 39.37007874015748143 ) ;
#9943 = VERTEX_POINT ( 'NONE', #766 ) ;
#9944 = ORIENTED_EDGE ( 'NONE', *, *, #13531, .T. ) ;
#9945 = EDGE_LOOP ( 'NONE', ( #7864, #2875 ) ) ;
#9946 = EDGE_LOOP ( 'NONE', ( #7334, #6314, #14754, #4635 ) ) ;
#9947 = AXIS2_PLACEMENT_3D ( 'NONE', #4219, #843, #6484 ) ;
#9948 = ORIENTED_EDGE ( 'NONE', *, *, #2251, .T. ) ;
#9949 = AXIS2_PLACEMENT_3D ( 'NONE', #11694, #8000, #11773 ) ;
#9950 = DIRECTION ( 'NONE',  ( 0.8660254037844383745, 0.000000000000000000, -0.5000000000000004441 ) ) ;
#9951 = PRODUCT_DEFINITION_SHAPE ( 'NONE', 'NONE',  #15479 ) ;
#9952 = DIRECTION ( 'NONE',  ( -0.000000000000000000, -1.000000000000000000, -0.000000000000000000 ) ) ;
#9953 = EDGE_CURVE ( 'NONE', #12689, #13646, #7738, .T. ) ;
#9954 = DIRECTION ( 'NONE',  ( -1.000000000000000000, 0.000000000000000000, 0.000000000000000000 ) ) ;
#9955 = AXIS2_PLACEMENT_3D ( 'NONE', #13641, #14904, #3055 ) ;
#9956 = DIRECTION ( 'NONE',  ( 0.000000000000000000, 0.000000000000000000, -1.000000000000000000 ) ) ;
#9957 = CARTESIAN_POINT ( 'NONE',  ( -1.185589860597406675, 0.3351407497376039935, 0.05695314934232943715 ) ) ;
#9958 = CARTESIAN_POINT ( 'NONE',  ( -1.871969607273682001, -2.941194614679324637, -0.05413282885976344189 ) ) ;
#9959 = VERTEX_POINT ( 'NONE', #12528 ) ;
#9960 = CARTESIAN_POINT ( 'NONE',  ( -2.073793831555620137, -2.576344762739053884, -0.1326668340855626793 ) ) ;
#9961 = CARTESIAN_POINT ( 'NONE',  ( -1.496171808639726875, 0.2144740403064262779, -0.03937007874015747977 ) ) ;
#9962 = AXIS2_PLACEMENT_3D ( 'NONE', #592, #10235, #12510 ) ;
#9963 = DIRECTION ( 'NONE',  ( 0.000000000000000000, 0.000000000000000000, -1.000000000000000000 ) ) ;
#9964 = ORIENTED_EDGE ( 'NONE', *, *, #8925, .F. ) ;
#9965 = ORIENTED_EDGE ( 'NONE', *, *, #8775, .F. ) ;
#9966 = EDGE_LOOP ( 'NONE', ( #4550, #11054, #2491, #10608 ) ) ;
#9967 = CIRCLE ( 'NONE', #8465, 0.01968503937007875723 ) ;
#9968 = CARTESIAN_POINT ( 'NONE',  ( -0.3441669734936866343, 2.010494531933507467, 0.05905511811023622659 ) ) ;
#9969 = DIRECTION ( 'NONE',  ( -1.000000000000000000, 0.000000000000000000, 0.000000000000000000 ) ) ;
#9970 = CIRCLE ( 'NONE', #1461, 0.003937007874015750579 ) ;
#9971 = CARTESIAN_POINT ( 'NONE',  ( -1.527714331928839098, 0.2380340132385416752, -0.03937007874015747977 ) ) ;
#9972 = CARTESIAN_POINT ( 'NONE',  ( -0.004184981454871861475, -0.1778800751599175500, -0.007038468095567116702 ) ) ;
#9973 = EDGE_LOOP ( 'NONE', ( #15313, #10630, #2419, #9183 ) ) ;
#9974 = DIRECTION ( 'NONE',  ( -0.8660254037844431485, 0.000000000000000000, -0.4999999999999918954 ) ) ;
#9975 = DIRECTION ( 'NONE',  ( 0.000000000000000000, 0.000000000000000000, -1.000000000000000000 ) ) ;
#9976 = LINE ( 'NONE', #8868, #14224 ) ;
#9977 = EDGE_CURVE ( 'NONE', #8823, #11277, #1788, .T. ) ;
#9978 = FACE_OUTER_BOUND ( 'NONE', #1710, .T. ) ;
#9979 = AXIS2_PLACEMENT_3D ( 'NONE', #9493, #2340, #14332 ) ;
#9980 = VERTEX_POINT ( 'NONE', #7664 ) ;
#9981 = ORIENTED_EDGE ( 'NONE', *, *, #9534, .T. ) ;
#9982 = ORIENTED_EDGE ( 'NONE', *, *, #7525, .T. ) ;
#9983 = FACE_OUTER_BOUND ( 'NONE', #8757, .T. ) ;
#9984 = CARTESIAN_POINT ( 'NONE',  ( 0.05905511811029064834, -0.1023622047244094474, -0.5870514566507987197 ) ) ;
#9985 = CARTESIAN_POINT ( 'NONE',  ( -0.06997329305369037744, 0.1451708428228665193, -0.05905511811023622659 ) ) ;
#9986 = DIRECTION ( 'NONE',  ( -1.000000000000000000, 0.000000000000000000, 0.000000000000000000 ) ) ;
#9987 = CARTESIAN_POINT ( 'NONE',  ( -1.400886410084237976, -0.004134161352976360726, 0.05905511811021026125 ) ) ;
#9988 = ADVANCED_FACE ( 'NONE', ( #13845 ), #5921, .T. ) ;
#9989 = CARTESIAN_POINT ( 'NONE',  ( -0.06692913385815749128, -0.4881889763779528324, -0.2377126739438355507 ) ) ;
#9990 = CARTESIAN_POINT ( 'NONE',  ( -1.596030944582063960, 0.1136756404979307328, 0.04477369844320258641 ) ) ;
#9991 = DIRECTION ( 'NONE',  ( -0.000000000000000000, 0.000000000000000000, 1.000000000000000000 ) ) ;
#9992 = EDGE_CURVE ( 'NONE', #11698, #14663, #12454, .T. ) ;
#9993 = DIRECTION ( 'NONE',  ( 0.000000000000000000, 0.000000000000000000, 1.000000000000000000 ) ) ;
#9994 = ORIENTED_EDGE ( 'NONE', *, *, #11199, .F. ) ;
#9995 = VERTEX_POINT ( 'NONE', #6627 ) ;
#9996 = VERTEX_POINT ( 'NONE', #1720 ) ;
#9997 = EDGE_CURVE ( 'NONE', #8022, #10241, #13945, .T. ) ;
#9998 = CARTESIAN_POINT ( 'NONE',  ( -1.959271706435208760, -2.897791574176610485, 0.1046970101888178434 ) ) ;
#9999 =( LENGTH_UNIT ( ) NAMED_UNIT ( * ) SI_UNIT ( $, .METRE. ) );
#10000 = EDGE_CURVE ( 'NONE', #3536, #7254, #10443, .T. ) ;
#10001 = DIRECTION ( 'NONE',  ( 0.000000000000000000, 0.000000000000000000, -1.000000000000000000 ) ) ;
#10002 = CARTESIAN_POINT ( 'NONE',  ( 0.4765556591343756976, 1.037732670558541903, 0.3487844890897296435 ) ) ;
#10003 = LINE ( 'NONE', #687, #5562 ) ;
#10004 = CARTESIAN_POINT ( 'NONE',  ( 0.000000000000000000, 0.3622047244094487306, 0.000000000000000000 ) ) ;
#10005 = CARTESIAN_POINT ( 'NONE',  ( -0.002500327830563101039, -0.1605493263772690415, 0.000000000000000000 ) ) ;
#10006 = EDGE_CURVE ( 'NONE', #14974, #10309, #10312, .T. ) ;
#10007 = DIRECTION ( 'NONE',  ( -0.000000000000000000, -0.000000000000000000, -1.000000000000000000 ) ) ;
#10008 = CARTESIAN_POINT ( 'NONE',  ( 0.1181102362204724532, 2.637795275590551825, 0.03937007874015747977 ) ) ;
#10009 = EDGE_CURVE ( 'NONE', #11649, #4524, #15030, .T. ) ;
#10010 = VERTEX_POINT ( 'NONE', #4280 ) ;
#10011 = ORIENTED_EDGE ( 'NONE', *, *, #5234, .F. ) ;
#10012 = ORIENTED_EDGE ( 'NONE', *, *, #636, .T. ) ;
#10013 = ORIENTED_EDGE ( 'NONE', *, *, #12581, .T. ) ;
#10014 = EDGE_LOOP ( 'NONE', ( #6833, #4943 ) ) ;
#10015 = CARTESIAN_POINT ( 'NONE',  ( -1.401202394148545194, -0.004217627448835788682, -0.05905511811023622659 ) ) ;
#10016 = DIRECTION ( 'NONE',  ( 0.000000000000000000, -0.2873478855663456066, -0.9578262852211513190 ) ) ;
#10017 = CARTESIAN_POINT ( 'NONE',  ( -2.184126211765464287, -1.725292181286298021, 0.08417626406393743932 ) ) ;
#10018 = FACE_OUTER_BOUND ( 'NONE', #6738, .T. ) ;
#10019 = DIRECTION ( 'NONE',  ( -1.000000000000000000, -0.000000000000000000, -3.476578583725179813E-16 ) ) ;
#10020 = CARTESIAN_POINT ( 'NONE',  ( 0.06278630405416070481, 1.038795175326500120, -0.5877245205702894548 ) ) ;
#10021 = CARTESIAN_POINT ( 'NONE',  ( -1.902950105202808606, -2.935536217473399212, -0.06922576094222421261 ) ) ;
#10022 = ORIENTED_EDGE ( 'NONE', *, *, #3600, .F. ) ;
#10023 = CYLINDRICAL_SURFACE ( 'NONE', #6168, 0.03937007874015751446 ) ;
#10024 = CARTESIAN_POINT ( 'NONE',  ( -0.5450083523900178806, 1.338582677165354395, 0.2464697422870344434 ) ) ;
#10025 = EDGE_CURVE ( 'NONE', #579, #9996, #6419, .T. ) ;
#10026 = CARTESIAN_POINT ( 'NONE',  ( -1.415146647999188767, -0.009757455497112661746, -0.06578125416968487460 ) ) ;
#10027 = EDGE_LOOP ( 'NONE', ( #9833, #11005, #14323, #8700 ) ) ;
#10028 = VERTEX_POINT ( 'NONE', #10017 ) ;
#10029 = EDGE_CURVE ( 'NONE', #12588, #7658, #7026, .T. ) ;
#10030 = UNCERTAINTY_MEASURE_WITH_UNIT (LENGTH_MEASURE( 1.000000000000000082E-05 ), #12326, 'distance_accuracy_value', 'NONE');
#10031 = VERTEX_POINT ( 'NONE', #12992 ) ;
#10032 = DIRECTION ( 'NONE',  ( 1.000000000000000000, 0.000000000000000000, 0.000000000000000000 ) ) ;
#10033 = CARTESIAN_POINT ( 'NONE',  ( -0.09948011493072102251, -0.4881889763779528324, -0.2443248468741946733 ) ) ;
#10034 = DIRECTION ( 'NONE',  ( -1.000000000000000000, -0.000000000000000000, 0.000000000000000000 ) ) ;
#10035 = CARTESIAN_POINT ( 'NONE',  ( 0.000000000000000000, 0.003937007874015860734, 0.000000000000000000 ) ) ;
#10036 = CARTESIAN_POINT ( 'NONE',  ( -1.596030944582063960, 0.1136756404979308160, 0.05905511811023622659 ) ) ;
#10037 = ORIENTED_EDGE ( 'NONE', *, *, #4172, .F. ) ;
#10038 = LINE ( 'NONE', #11130, #12190 ) ;
#10039 = FACE_OUTER_BOUND ( 'NONE', #1939, .T. ) ;
#10040 = SPHERICAL_SURFACE ( 'NONE', #8217, 0.003937007874015747977 ) ;
#10041 = CARTESIAN_POINT ( 'NONE',  ( -0.1552072824047652233, -0.003937007874015747977, -0.5870514566507987197 ) ) ;
#10042 = DIRECTION ( 'NONE',  ( 0.8660254037844389297, 0.000000000000000000, -0.4999999999999994449 ) ) ;
#10043 = ORIENTED_EDGE ( 'NONE', *, *, #11469, .T. ) ;
#10044 = ORIENTED_EDGE ( 'NONE', *, *, #4614, .F. ) ;
#10045 = ORIENTED_EDGE ( 'NONE', *, *, #1026, .F. ) ;
#10046 = CARTESIAN_POINT ( 'NONE',  ( 0.000000000000000000, 1.653543307086614567, -0.5984251968503937480 ) ) ;
#10047 = CARTESIAN_POINT ( 'NONE',  ( -0.2393297813659119588, -0.1023622047244094474, 0.06089400679736759608 ) ) ;
#10048 = CARTESIAN_POINT ( 'NONE',  ( -0.2661821753646866906, -0.1023622047244094474, 0.03548265769538203052 ) ) ;
#10049 = DIRECTION ( 'NONE',  ( -0.8660254037844309360, 0.000000000000000000, 0.5000000000000134337 ) ) ;
#10050 = APPLICATION_PROTOCOL_DEFINITION ( 'draft international standard', 'automotive_design', 1998, #5986 ) ;
#10051 = CARTESIAN_POINT ( 'NONE',  ( -1.181102362204724310, 0.1240157480314959815, -0.02952755905511811330 ) ) ;
#10052 = CARTESIAN_POINT ( 'NONE',  ( -1.220472440944881720, 0.000000000000000000, -0.02559055118110236185 ) ) ;
#10053 = DIRECTION ( 'NONE',  ( 0.5000000000000004441, -1.502314598737161516E-14, 0.8660254037844384856 ) ) ;
#10054 = CARTESIAN_POINT ( 'NONE',  ( -0.1062992125983150127, -0.4881889763779528324, -0.2482618547482104143 ) ) ;
#10055 = B_SPLINE_CURVE_WITH_KNOTS ( 'NONE', 3,
 ( #2535, #9688, #14375, #2615, #1455, #4891, #13347, #6132 ),
 .UNSPECIFIED., .F., .F.,
 ( 4, 2, 2, 4 ),
 ( 0.000000000000000000, 0.0004593534821998672391, 0.0009187069643997344782, 0.001837413928799469390 ),
 .UNSPECIFIED. ) ;
#10056 = CARTESIAN_POINT ( 'NONE',  ( 0.000000000000000000, -0.1023622047244094474, 0.000000000000000000 ) ) ;
#10057 = CARTESIAN_POINT ( 'NONE',  ( 0.000000000000000000, 1.377952755905512028, 0.7007874015748031260 ) ) ;
#10058 = ORIENTED_EDGE ( 'NONE', *, *, #6388, .T. ) ;
#10059 = EDGE_CURVE ( 'NONE', #6809, #6855, #2194, .T. ) ;
#10060 = ORIENTED_EDGE ( 'NONE', *, *, #778, .T. ) ;
#10061 = ADVANCED_FACE ( 'NONE', ( #8131 ), #2178, .T. ) ;
#10062 = ORIENTED_EDGE ( 'NONE', *, *, #10840, .T. ) ;
#10063 = ADVANCED_FACE ( 'NONE', ( #12757 ), #11814, .T. ) ;
#10064 = DIRECTION ( 'NONE',  ( 0.000000000000000000, 0.000000000000000000, 1.000000000000000000 ) ) ;
#10065 = CARTESIAN_POINT ( 'NONE',  ( -1.951481176069858270, -2.917150509235289846, -0.07712466264118481019 ) ) ;
#10066 = FACE_OUTER_BOUND ( 'NONE', #5804, .T. ) ;
#10067 = CARTESIAN_POINT ( 'NONE',  ( -1.990389617432203551, -2.816408247477061089, -0.1718103083736243208 ) ) ;
#10068 = DIRECTION ( 'NONE',  ( -0.000000000000000000, -2.212657494868377674E-16, -1.000000000000000000 ) ) ;
#10069 = DIRECTION ( 'NONE',  ( 0.000000000000000000, -0.000000000000000000, -1.000000000000000000 ) ) ;
#10070 = CARTESIAN_POINT ( 'NONE',  ( -1.879797169039889582, -2.922016187845676960, -0.01134394994210854990 ) ) ;
#10071 = CARTESIAN_POINT ( 'NONE',  ( 0.4342073824196633347, -0.09448818897637796532, 0.4299076816772810505 ) ) ;
#10072 = CARTESIAN_POINT ( 'NONE',  ( -2.084730511138506159, -1.679593886630597277, -0.08366141732295870326 ) ) ;
#10073 = AXIS2_PLACEMENT_3D ( 'NONE', #8043, #2254, #15263 ) ;
#10074 = VERTEX_POINT ( 'NONE', #8040 ) ;
#10075 = EDGE_CURVE ( 'NONE', #14099, #12256, #4187, .T. ) ;
#10076 = TOROIDAL_SURFACE ( 'NONE', #3324, 0.04330708661417329020, 0.003937007874015747977 ) ;
#10077 = ORIENTED_EDGE ( 'NONE', *, *, #12977, .T. ) ;
#10078 = VERTEX_POINT ( 'NONE', #6781 ) ;
#10079 = ADVANCED_FACE ( 'NONE', ( #11660 ), #10637, .T. ) ;
#10080 = ORIENTED_EDGE ( 'NONE', *, *, #9464, .F. ) ;
#10081 = VERTEX_POINT ( 'NONE', #9475 ) ;
#10082 = CARTESIAN_POINT ( 'NONE',  ( -1.417043596213071632, -0.04217320660662462334, -0.06809929043877624433 ) ) ;
#10083 = ADVANCED_FACE ( 'NONE', ( #5689 ), #3512, .F. ) ;
#10084 = DIRECTION ( 'NONE',  ( -0.5000000000000001110, 0.000000000000000000, 0.8660254037844385966 ) ) ;
#10085 = CARTESIAN_POINT ( 'NONE',  ( -0.4788739157331333707, -0.09842519685039370636, 0.3446689608323532106 ) ) ;
#10086 = AXIS2_PLACEMENT_3D ( 'NONE', #9662, #7222, #8311 ) ;
#10087 = CONICAL_SURFACE ( 'NONE', #584, 0.08858267716535432601, 1.047197551196600074 ) ;
#10088 = DIRECTION ( 'NONE',  ( 0.000000000000000000, 0.000000000000000000, 1.000000000000000000 ) ) ;
#10089 = CIRCLE ( 'NONE', #10343, 0.003937007874015724558 ) ;
#10090 = DIRECTION ( 'NONE',  ( -0.8660254037844385966, 0.000000000000000000, -0.5000000000000002220 ) ) ;
#10091 = DIRECTION ( 'NONE',  ( 0.000000000000000000, 1.000000000000000000, 0.000000000000000000 ) ) ;
#10092 = CIRCLE ( 'NONE', #6305, 0.003937007874015754916 ) ;
#10093 = DIRECTION ( 'NONE',  ( 1.000000000000000000, 0.000000000000000000, 0.000000000000000000 ) ) ;
#10094 = CARTESIAN_POINT ( 'NONE',  ( -1.180847381073178770, 0.3433074774414748287, 0.04453711288976135857 ) ) ;
#10095 = CARTESIAN_POINT ( 'NONE',  ( -1.903002266451024216, -2.935391651063040008, 0.06956102793678921314 ) ) ;
#10096 = ORIENTED_EDGE ( 'NONE', *, *, #6715, .F. ) ;
#10097 = FACE_OUTER_BOUND ( 'NONE', #12198, .T. ) ;
#10098 = ORIENTED_EDGE ( 'NONE', *, *, #14036, .T. ) ;
#10099 = ORIENTED_EDGE ( 'NONE', *, *, #6234, .T. ) ;
#10100 = AXIS2_PLACEMENT_3D ( 'NONE', #4360, #3266, #8037 ) ;
#10101 = CIRCLE ( 'NONE', #12356, 0.03937007874015753528 ) ;
#10102 = ADVANCED_FACE ( 'NONE', ( #4519 ), #11898, .T. ) ;
#10103 = AXIS2_PLACEMENT_3D ( 'NONE', #14750, #3927, #4069 ) ;
#10104 = AXIS2_PLACEMENT_3D ( 'NONE', #12497, #7474, #1525 ) ;
#10105 = ORIENTED_EDGE ( 'NONE', *, *, #7498, .F. ) ;
#10106 = CARTESIAN_POINT ( 'NONE',  ( 0.000000000000000000, 0.5826771653543306728, -0.7086614173228346081 ) ) ;
#10107 = ADVANCED_FACE ( 'NONE', ( #150 ), #1473, .T. ) ;
#10108 = EDGE_CURVE ( 'NONE', #579, #13379, #9463, .T. ) ;
#10109 = DIRECTION ( 'NONE',  ( 0.4999999999999922284, -0.000000000000000000, -0.8660254037844431485 ) ) ;
#10110 = DIRECTION ( 'NONE',  ( 1.000000000000000000, 0.000000000000000000, 3.476578583725179813E-16 ) ) ;
#10111 = CARTESIAN_POINT ( 'NONE',  ( -1.527714331928839098, 0.2380340132385416752, 0.03937007874015747977 ) ) ;
#10112 = VECTOR ( 'NONE', #12455, 39.37007874015748143 ) ;
#10113 = DIRECTION ( 'NONE',  ( 0.000000000000000000, 0.000000000000000000, 1.000000000000000000 ) ) ;
#10114 = AXIS2_PLACEMENT_3D ( 'NONE', #11940, #12015, #2285 ) ;
#10115 = LINE ( 'NONE', #8861, #3135 ) ;
#10116 = VERTEX_POINT ( 'NONE', #1534 ) ;
#10117 = CYLINDRICAL_SURFACE ( 'NONE', #7669, 0.7086614173228346081 ) ;
#10118 = VECTOR ( 'NONE', #2614, 39.37007874015748143 ) ;
#10119 = ADVANCED_FACE ( 'NONE', ( #14544 ), #2718, .F. ) ;
#10120 = CARTESIAN_POINT ( 'NONE',  ( -0.4859532342797812654, 1.338582677165354395, 0.3487562073009442543 ) ) ;
#10121 = AXIS2_PLACEMENT_3D ( 'NONE', #545, #13854, #5296 ) ;
#10122 = AXIS2_PLACEMENT_3D ( 'NONE', #2764, #7534, #10831 ) ;
#10123 = CARTESIAN_POINT ( 'NONE',  ( -1.417802900492933560, -0.04287136159519130962, -0.06853082236355059753 ) ) ;
#10124 = CYLINDRICAL_SURFACE ( 'NONE', #7583, 0.003937007874015724558 ) ;
#10125 = AXIS2_PLACEMENT_3D ( 'NONE', #2471, #7308, #9528 ) ;
#10126 = CARTESIAN_POINT ( 'NONE',  ( -0.05905511811023622659, 1.043307086614173151, -0.8267716535433072833 ) ) ;
#10127 = ORIENTED_EDGE ( 'NONE', *, *, #6432, .F. ) ;
#10129 = EDGE_LOOP ( 'NONE', ( #15312, #11105, #14255, #13597 ) ) ;
#10128 = AXIS2_PLACEMENT_3D ( 'NONE', #12794, #6915, #11710 ) ;
#10130 = AXIS2_PLACEMENT_3D ( 'NONE', #1831, #8898, #9925 ) ;
#10131 = VECTOR ( 'NONE', #745, 39.37007874015748143 ) ;
#10132 = DIRECTION ( 'NONE',  ( 1.669238443041289155E-16, -0.000000000000000000, 1.000000000000000000 ) ) ;
#10133 = DIRECTION ( 'NONE',  ( -0.8660254037844385966, 0.000000000000000000, -0.5000000000000000000 ) ) ;
#10134 = CARTESIAN_POINT ( 'NONE',  ( -1.574484809660414042, 0.1100025355989073528, 0.06175692796217682051 ) ) ;
#10135 = SHAPE_DEFINITION_REPRESENTATION ( #5766, #12105 ) ;
#10136 = DIRECTION ( 'NONE',  ( 0.000000000000000000, 0.000000000000000000, -1.000000000000000000 ) ) ;
#10137 = DIRECTION ( 'NONE',  ( -1.000000000000000000, 0.000000000000000000, 0.000000000000000000 ) ) ;
#10138 = CARTESIAN_POINT ( 'NONE',  ( 0.1022864650139100745, 0.05905511811023622659, 1.563012696487738457E-17 ) ) ;
#10139 = EDGE_CURVE ( 'NONE', #624, #4871, #12275, .T. ) ;
#10140 = CYLINDRICAL_SURFACE ( 'NONE', #12636, 0.003937007874015749712 ) ;
#10141 = VECTOR ( 'NONE', #5402, 39.37007874015748143 ) ;
#10142 = AXIS2_PLACEMENT_3D ( 'NONE', #5259, #9991, #13750 ) ;
#10143 = AXIS2_PLACEMENT_3D ( 'NONE', #12890, #2160, #1224 ) ;
#10144 = CARTESIAN_POINT ( 'NONE',  ( 1.181102362204724310, 4.044111181948214319E-16, 0.02952755905511811330 ) ) ;
#10145 = VERTEX_POINT ( 'NONE', #4911 ) ;
#10146 = CIRCLE ( 'NONE', #13643, 0.003937007874015721089 ) ;
#10147 = ORIENTED_EDGE ( 'NONE', *, *, #2735, .T. ) ;
#10148 = DIRECTION ( 'NONE',  ( 0.000000000000000000, 0.000000000000000000, -1.000000000000000000 ) ) ;
#10149 = EDGE_LOOP ( 'NONE', ( #1777, #3281, #10776, #3750 ) ) ;
#10150 = ORIENTED_EDGE ( 'NONE', *, *, #12210, .F. ) ;
#10151 = AXIS2_PLACEMENT_3D ( 'NONE', #3188, #12258, #8646 ) ;
#10152 = VECTOR ( 'NONE', #3586, 39.37007874015748143 ) ;
#10153 = CARTESIAN_POINT ( 'NONE',  ( 0.000000000000000000, 0.07480314960629921850, 0.000000000000000000 ) ) ;
#10154 = CARTESIAN_POINT ( 'NONE',  ( -1.994705189605018303, -2.804563710229789564, 0.1744288432568320280 ) ) ;
#10155 =( CONVERSION_BASED_UNIT ( 'INCH', #7871 ) LENGTH_UNIT ( ) NAMED_UNIT ( #11555 ) );
#10156 = AXIS2_PLACEMENT_3D ( 'NONE', #9289, #11801, #14151 ) ;
#10157 = DIRECTION ( 'NONE',  ( 1.000000000000000000, 0.000000000000000000, 0.000000000000000000 ) ) ;
#10158 = CARTESIAN_POINT ( 'NONE',  ( -0.05905511811023622659, 1.190944881889763884, -0.8267716535433072833 ) ) ;
#10159 = CARTESIAN_POINT ( 'NONE',  ( 4.821444091131311524E-18, 0.4094488188976377896, 0.03937007874015747977 ) ) ;
#10160 = FACE_OUTER_BOUND ( 'NONE', #3569, .T. ) ;
#10161 = CARTESIAN_POINT ( 'NONE',  ( 0.1754240695251997051, -0.1023622047244094474, 0.1694721104386522070 ) ) ;
#10162 = CARTESIAN_POINT ( 'NONE',  ( 0.000000000000000000, 1.338582677165354395, 0.000000000000000000 ) ) ;
#10163 = AXIS2_PLACEMENT_3D ( 'NONE', #3304, #4245, #6666 ) ;
#10164 = AXIS2_PLACEMENT_3D ( 'NONE', #10305, #6699, #13920 ) ;
#10165 = ORIENTED_EDGE ( 'NONE', *, *, #10937, .T. ) ;
#10166 = EDGE_CURVE ( 'NONE', #880, #1514, #2942, .T. ) ;
#10167 = ORIENTED_EDGE ( 'NONE', *, *, #10029, .T. ) ;
#10168 = ORIENTED_EDGE ( 'NONE', *, *, #7027, .T. ) ;
#10169 = AXIS2_PLACEMENT_3D ( 'NONE', #7064, #13978, #3244 ) ;
#10170 = EDGE_LOOP ( 'NONE', ( #11753, #9281, #13999, #6091 ) ) ;
#10171 = ORIENTED_EDGE ( 'NONE', *, *, #378, .T. ) ;
#10172 = CARTESIAN_POINT ( 'NONE',  ( 8.582170482213735190E-17, 1.645669291338583085, 0.7007874015748031260 ) ) ;
#10173 = CARTESIAN_POINT ( 'NONE',  ( 0.000000000000000000, 0.4133858267716535306, 0.000000000000000000 ) ) ;
#10174 = CYLINDRICAL_SURFACE ( 'NONE', #7439, 0.03937007874015751446 ) ;
#10175 = DIRECTION ( 'NONE',  ( 0.000000000000000000, -1.734723475976806463E-14, -1.000000000000000000 ) ) ;
#10176 = DIRECTION ( 'NONE',  ( 0.000000000000000000, 0.000000000000000000, 1.000000000000000000 ) ) ;
#10177 = DIRECTION ( 'NONE',  ( -0.000000000000000000, -1.000000000000000000, 0.000000000000000000 ) ) ;
#10178 = FACE_OUTER_BOUND ( 'NONE', #7332, .T. ) ;
#10179 = CIRCLE ( 'NONE', #680, 0.007874015748031516770 ) ;
#10180 = CARTESIAN_POINT ( 'NONE',  ( -0.5615510810874360104, -0.09842519685039370636, 0.2014679098129269208 ) ) ;
#10181 = EDGE_CURVE ( 'NONE', #3768, #4146, #4688, .T. ) ;
#10182 = ORIENTED_EDGE ( 'NONE', *, *, #7232, .F. ) ;
#10183 = DIRECTION ( 'NONE',  ( 0.8660254037844388186, 0.000000000000000000, -0.4999999999999996669 ) ) ;
#10184 = ORIENTED_EDGE ( 'NONE', *, *, #10009, .T. ) ;
#10185 = EDGE_CURVE ( 'NONE', #4812, #11006, #10783, .T. ) ;
#10186 =( BOUNDED_SURFACE ( )  B_SPLINE_SURFACE ( 3, 2, ( 
 ( #13303, #10963, #12294 ),
 ( #1554, #6307, #11103 ),
 ( #9957, #7570, #8767 ),
 ( #2016, #5382, #14881 ),
 ( #9008, #5292, #10094 ),
 ( #13617, #4141, #5463 ) ),
 .UNSPECIFIED., .F., .F., .T. ) 
 B_SPLINE_SURFACE_WITH_KNOTS ( ( 4, 2, 4 ),
 ( 3, 3 ),
 ( -3.623019766863768071E-05, 0.0007449614524472654561, 0.001526153102563168606 ),
 ( 0.000000000000000000, 1.000000000000000000 ),
 .UNSPECIFIED. ) 
 GEOMETRIC_REPRESENTATION_ITEM ( )  RATIONAL_B_SPLINE_SURFACE ( (
 ( 1.000000000000000000, 1.000000000000000000, 1.000000000000000000),
 ( 1.000000000000000000, 1.000000656565393609, 1.000000000000000000),
 ( 1.000000000000000000, 0.9999739034943005977, 1.000000000000000000),
 ( 1.000000000000000000, 0.9999216474068165494, 1.000000000000000000),
 ( 1.000000000000000000, 0.9998986130898321889, 1.000000000000000000),
 ( 1.000000000000000000, 0.9998995914418479236, 1.000000000000000000) ) ) 
 REPRESENTATION_ITEM ( '' )  SURFACE ( )  );
#10187 = ORIENTED_EDGE ( 'NONE', *, *, #4032, .T. ) ;
#10188 = AXIS2_PLACEMENT_3D ( 'NONE', #15306, #4565, #9351 ) ;
#10189 = UNCERTAINTY_MEASURE_WITH_UNIT (LENGTH_MEASURE( 1.000000000000000082E-05 ), #13101, 'distance_accuracy_value', 'NONE');
#10190 = ORIENTED_EDGE ( 'NONE', *, *, #9854, .T. ) ;
#10191 = CIRCLE ( 'NONE', #12700, 0.04330708661417326938 ) ;
#10192 = AXIS2_PLACEMENT_3D ( 'NONE', #7753, #8152, #13165 ) ;
#10193 = DIRECTION ( 'NONE',  ( 0.8660254037844374864, 0.000000000000000000, 0.5000000000000017764 ) ) ;
#10194 = CARTESIAN_POINT ( 'NONE',  ( 0.7114373258145217926, 1.190944881889763884, 0.3425575548946133142 ) ) ;
#10195 = CARTESIAN_POINT ( 'NONE',  ( 0.000000000000000000, 0.06496062992125986590, 0.04527559055118110520 ) ) ;
#10197 = AXIS2_PLACEMENT_3D ( 'NONE', #14196, #12720, #8163 ) ;
#10196 = CARTESIAN_POINT ( 'NONE',  ( 0.1552072824047652233, -0.09448818897637796532, -0.5909884645248143498 ) ) ;
#10198 = CARTESIAN_POINT ( 'NONE',  ( 0.4307978335858663188, -0.003937007874015747977, 0.4279391777402731800 ) ) ;
#10199 = EDGE_CURVE ( 'NONE', #7217, #3033, #15448, .T. ) ;
#10200 = VERTEX_POINT ( 'NONE', #229 ) ;
#10201 = DIRECTION ( 'NONE',  ( 0.8660254037844385966, 0.000000000000000000, 0.5000000000000000000 ) ) ;
#10202 = PRESENTATION_LAYER_ASSIGNMENT (  '', '', ( #3202 ) ) ;
#10203 = DIRECTION ( 'NONE',  ( 0.000000000000000000, -4.956352788505160310E-16, -1.000000000000000000 ) ) ;
#10204 = CYLINDRICAL_SURFACE ( 'NONE', #3090, 0.003937007874015747109 ) ;
#10205 = ORIENTED_EDGE ( 'NONE', *, *, #12678, .F. ) ;
#10206 = ADVANCED_FACE ( 'NONE', ( #7259 ), #1309, .T. ) ;
#10207 = DIRECTION ( 'NONE',  ( 0.5000000000000001110, 0.000000000000000000, 0.8660254037844384856 ) ) ;
#10208 = ADVANCED_FACE ( 'NONE', ( #13287 ), #1244, .T. ) ;
#10209 = VERTEX_POINT ( 'NONE', #12048 ) ;
#10210 = ORIENTED_EDGE ( 'NONE', *, *, #10665, .F. ) ;
#10211 = AXIS2_PLACEMENT_3D ( 'NONE', #12209, #11079, #64 ) ;
#10212 =( REPRESENTATION_RELATIONSHIP ('NONE','NONE', #8904, #2403 ) REPRESENTATION_RELATIONSHIP_WITH_TRANSFORMATION ( #7937 )SHAPE_REPRESENTATION_RELATIONSHIP( ) );
#10213 = EDGE_CURVE ( 'NONE', #9905, #851, #6061, .T. ) ;
#10214 = DIRECTION ( 'NONE',  ( -0.000000000000000000, 1.000000000000000000, -0.000000000000000000 ) ) ;
#10215 = CIRCLE ( 'NONE', #13221, 0.003937007874015721089 ) ;
#10216 = FACE_OUTER_BOUND ( 'NONE', #6496, .T. ) ;
#10217 = CYLINDRICAL_SURFACE ( 'NONE', #6854, 0.007874015748031516770 ) ;
#10218 = SHAPE_DEFINITION_REPRESENTATION ( #914, #2403 ) ;
#10219 = CARTESIAN_POINT ( 'NONE',  ( 0.000000000000000000, 1.614173228346457156, 0.6614173228346456046 ) ) ;
#10220 = SPHERICAL_SURFACE ( 'NONE', #7122, 0.003937007874015747977 ) ;
#10221 = EDGE_LOOP ( 'NONE', ( #3588, #4750, #4648 ) ) ;
#10222 = CARTESIAN_POINT ( 'NONE',  ( -2.068647409231313183, -2.591269129772357349, -0.1345927733208679422 ) ) ;
#10223 = DIRECTION ( 'NONE',  ( 0.000000000000000000, 0.000000000000000000, -1.000000000000000000 ) ) ;
#10224 = CARTESIAN_POINT ( 'NONE',  ( 0.4861941749621881415, 1.338582677165354395, 0.3488953144687809704 ) ) ;
#10225 = ADVANCED_FACE ( 'NONE', ( #6222 ), #10856, .T. ) ;
#10226 = ORIENTED_EDGE ( 'NONE', *, *, #15345, .F. ) ;
#10227 = ORIENTED_EDGE ( 'NONE', *, *, #10006, .F. ) ;
#10228 = CARTESIAN_POINT ( 'NONE',  ( 6.846450609406462919E-17, 0.5511811023622046335, -0.5590551181102362266 ) ) ;
#10229 = ORIENTED_EDGE ( 'NONE', *, *, #8552, .T. ) ;
#10230 = EDGE_CURVE ( 'NONE', #13695, #2668, #217, .T. ) ;
#10231 = ORIENTED_EDGE ( 'NONE', *, *, #2238, .F. ) ;
#10232 = ADVANCED_FACE ( 'NONE', ( #2547 ), #1206, .T. ) ;
#10233 = DIRECTION ( 'NONE',  ( 0.4999999999999998335, 0.000000000000000000, 0.8660254037844388186 ) ) ;
#10234 = CARTESIAN_POINT ( 'NONE',  ( -1.996856552776540505, -2.798603954469058852, 0.1754249698848522609 ) ) ;
#10235 = DIRECTION ( 'NONE',  ( -0.5000000000000039968, 0.000000000000000000, -0.8660254037844362651 ) ) ;
#10236 = CARTESIAN_POINT ( 'NONE',  ( -1.971194147208129355, -2.816470572534745198, -0.1716880295712622795 ) ) ;
#10237 = DIRECTION ( 'NONE',  ( 0.000000000000000000, -1.000000000000000000, 0.000000000000000000 ) ) ;
#10238 = DIRECTION ( 'NONE',  ( 0.000000000000000000, 0.000000000000000000, 1.000000000000000000 ) ) ;
#10239 = DIRECTION ( 'NONE',  ( 0.000000000000000000, 0.000000000000000000, -1.000000000000000000 ) ) ;
#10240 = CARTESIAN_POINT ( 'NONE',  ( -2.046873694507677754, -2.382074652208439058, -0.1339202096237949169 ) ) ;
#10241 = VERTEX_POINT ( 'NONE', #5042 ) ;
#10242 = VERTEX_POINT ( 'NONE', #5131 ) ;
#10243 = VERTEX_POINT ( 'NONE', #11985 ) ;
#10244 = ORIENTED_EDGE ( 'NONE', *, *, #10888, .F. ) ;
#10245 = CARTESIAN_POINT ( 'NONE',  ( 9.360245101547351149E-18, 0.07093549527207514138, 0.07900545476875124595 ) ) ;
#10246 = CARTESIAN_POINT ( 'NONE',  ( -0.1574803149606299191, 0.03937007874015749365, 0.000000000000000000 ) ) ;
#10247 = CARTESIAN_POINT ( 'NONE',  ( -0.5894146648244306119, -0.09842519685039370636, 0.1610807828475335490 ) ) ;
#10248 = CARTESIAN_POINT ( 'NONE',  ( 0.03886060139087953863, 0.07874015748031495954, 0.08219815605943972536 ) ) ;
#10249 = FACE_OUTER_BOUND ( 'NONE', #5824, .T. ) ;
#10250 = CARTESIAN_POINT ( 'NONE',  ( -1.293236445124221312, 0.1355266887446167634, 0.03937007874015747977 ) ) ;
#10251 = CARTESIAN_POINT ( 'NONE',  ( -1.181102362204724310, 0.000000000000000000, 0.02559055118110236185 ) ) ;
#10252 = CARTESIAN_POINT ( 'NONE',  ( -1.926777348550824165, -2.867314143461890730, -0.1500590184085016932 ) ) ;
#10253 = VERTEX_POINT ( 'NONE', #5353 ) ;
#10254 = DIRECTION ( 'NONE',  ( -1.000000000000000000, 0.000000000000000000, 0.000000000000000000 ) ) ;
#10255 = CARTESIAN_POINT ( 'NONE',  ( -0.4305093106511125312, -0.2952755905511811330, 0.1712715594937239405 ) ) ;
#10256 = VERTEX_POINT ( 'NONE', #5206 ) ;
#10257 = ORIENTED_EDGE ( 'NONE', *, *, #10687, .F. ) ;
#10258 = ADVANCED_FACE ( 'NONE', ( #6461 ), #6606, .T. ) ;
#10259 = ORIENTED_EDGE ( 'NONE', *, *, #5600, .T. ) ;
#10260 = EDGE_CURVE ( 'NONE', #4871, #15235, #12220, .T. ) ;
#10261 = CARTESIAN_POINT ( 'NONE',  ( -0.1062992125983150959, -0.09842519685039370636, -3.695575659861521121E-17 ) ) ;
#10262 = EDGE_CURVE ( 'NONE', #3552, #9161, #13583, .T. ) ;
#10263 = FACE_OUTER_BOUND ( 'NONE', #2922, .T. ) ;
#10264 = CARTESIAN_POINT ( 'NONE',  ( -0.4857119623810620679, 1.043292445042268257, 0.3486169089052708614 ) ) ;
#10265 = CYLINDRICAL_SURFACE ( 'NONE', #9200, 0.01968503937007875723 ) ;
#10266 = DIRECTION ( 'NONE',  ( 0.8660254037844388186, 0.000000000000000000, -0.4999999999999998335 ) ) ;
#10267 = DIRECTION ( 'NONE',  ( 0.8660254037844383745, 9.486769009248228879E-16, 0.5000000000000004441 ) ) ;
#10268 = EDGE_LOOP ( 'NONE', ( #2663, #4027, #6141, #11322 ) ) ;
#10269 = DIRECTION ( 'NONE',  ( 1.000000000000000000, 0.000000000000000000, 3.614007241618347785E-16 ) ) ;
#10270 = CARTESIAN_POINT ( 'NONE',  ( 0.000000000000000000, 2.433070866141732846, 0.000000000000000000 ) ) ;
#10271 = CYLINDRICAL_SURFACE ( 'NONE', #6189, 0.03937007874015754916 ) ;
#10272 = CARTESIAN_POINT ( 'NONE',  ( -1.063205505495480097, 0.7941372572243097228, 0.03937007874015747977 ) ) ;
#10273 = EDGE_LOOP ( 'NONE', ( #5896, #12441, #13016, #207 ) ) ;
#10274 = FACE_BOUND ( 'NONE', #10489, .T. ) ;
#10275 = ORIENTED_EDGE ( 'NONE', *, *, #5551, .F. ) ;
#10276 = EDGE_CURVE ( 'NONE', #10892, #7046, #5684, .T. ) ;
#10277 = VERTEX_POINT ( 'NONE', #5271 ) ;
#10278 = ADVANCED_FACE ( 'NONE', ( #10066 ), #6378, .F. ) ;
#10279 = ORIENTED_EDGE ( 'NONE', *, *, #9622, .T. ) ;
#10280 = CARTESIAN_POINT ( 'NONE',  ( 0.1638199706403873079, -0.4921259842519685179, 0.2127791970528254417 ) ) ;
#10281 = FACE_BOUND ( 'NONE', #3410, .T. ) ;
#10282 = EDGE_CURVE ( 'NONE', #11838, #11452, #13212, .T. ) ;
#10283 = CARTESIAN_POINT ( 'NONE',  ( 0.000000000000000000, 0.000000000000000000, -0.1574803149606299191 ) ) ;
#10284 = DIRECTION ( 'NONE',  ( 0.000000000000000000, 0.000000000000000000, 1.000000000000000000 ) ) ;
#10285 = CARTESIAN_POINT ( 'NONE',  ( 1.181102362204724310, 4.044111181948214319E-16, -0.02559055118110236185 ) ) ;
#10286 = DIRECTION ( 'NONE',  ( 0.5000000000000002220, 0.000000000000000000, 0.8660254037844384856 ) ) ;
#10287 = ORIENTED_EDGE ( 'NONE', *, *, #8077, .F. ) ;
#10288 = CARTESIAN_POINT ( 'NONE',  ( 0.000000000000000000, 0.04724409448818898960, 0.000000000000000000 ) ) ;
#10289 = DIRECTION ( 'NONE',  ( -3.614007241618347785E-16, 0.000000000000000000, 1.000000000000000000 ) ) ;
#10290 = CARTESIAN_POINT ( 'NONE',  ( -0.03886060139087894189, 0.000000000000000000, -0.08219815605944147396 ) ) ;
#10291 = ORIENTED_EDGE ( 'NONE', *, *, #13260, .F. ) ;
#10292 = ORIENTED_EDGE ( 'NONE', *, *, #5773, .F. ) ;
#10293 = CARTESIAN_POINT ( 'NONE',  ( 0.1022864650139100745, 0.05905511811023622659, 1.563012696487738457E-17 ) ) ;
#10294 = ORIENTED_EDGE ( 'NONE', *, *, #2629, .T. ) ;
#10295 = EDGE_LOOP ( 'NONE', ( #12070, #1782, #13711, #12780 ) ) ;
#10296 = CYLINDRICAL_SURFACE ( 'NONE', #13106, 0.1574803149606299191 ) ;
#10297 = CARTESIAN_POINT ( 'NONE',  ( -1.973162713238899135, -2.810427108646321503, 0.1731293751518992452 ) ) ;
#10298 =( NAMED_UNIT ( * ) PLANE_ANGLE_UNIT ( ) SI_UNIT ( $, .RADIAN. ) );
#10299 = ADVANCED_FACE ( 'NONE', ( #12578 ), #9472, .F. ) ;
#10300 = DIRECTION ( 'NONE',  ( 0.000000000000000000, 0.000000000000000000, -1.000000000000000000 ) ) ;
#10301 = DIRECTION ( 'NONE',  ( 0.000000000000000000, 1.000000000000000000, -0.000000000000000000 ) ) ;
#10302 = CARTESIAN_POINT ( 'NONE',  ( 0.09061599198715353243, 0.06736074103232449206, 0.007444810018878659542 ) ) ;
#10303 = EDGE_CURVE ( 'NONE', #15395, #5700, #1841, .T. ) ;
#10304 = LINE ( 'NONE', #12438, #1084 ) ;
#10305 = CARTESIAN_POINT ( 'NONE',  ( -1.431036756819011213, -0.02829858486107876200, 0.1968503937007874127 ) ) ;
#10306 = ORIENTED_EDGE ( 'NONE', *, *, #15163, .F. ) ;
#10307 = ORIENTED_EDGE ( 'NONE', *, *, #13036, .F. ) ;
#10308 = ORIENTED_EDGE ( 'NONE', *, *, #10276, .T. ) ;
#10309 = VERTEX_POINT ( 'NONE', #12666 ) ;
#10310 = CARTESIAN_POINT ( 'NONE',  ( -0.4769054117961255002, -0.4881889763779528324, 0.3480785096661502265 ) ) ;
#10311 = DIRECTION ( 'NONE',  ( 1.000000000000000000, 0.000000000000000000, 0.000000000000000000 ) ) ;
#10312 = LINE ( 'NONE', #10247, #13201 ) ;
#10313 = DIRECTION ( 'NONE',  ( 0.000000000000000000, 0.000000000000000000, 1.000000000000000000 ) ) ;
#10314 = CARTESIAN_POINT ( 'NONE',  ( -1.276200637803905691, -0.1988000726501942539, -0.03937007874015747977 ) ) ;
#10315 = CARTESIAN_POINT ( 'NONE',  ( 6.750021727583836750E-17, 0.000000000000000000, 0.5511811023622046335 ) ) ;
#10316 = DIRECTION ( 'NONE',  ( -1.000000000000000000, 0.000000000000000000, -9.020562075079388813E-13 ) ) ;
#10317 = EDGE_LOOP ( 'NONE', ( #6702, #4126, #2041, #9981, #10578, #10529, #5454, #6367, #1607, #7317, #10454, #3986, #14917, #13189, #14674, #1359, #5522, #14111 ) ) ;
#10318 = FACE_OUTER_BOUND ( 'NONE', #6987, .T. ) ;
#10319 = EDGE_CURVE ( 'NONE', #14035, #11638, #11464, .T. ) ;
#10320 = CARTESIAN_POINT ( 'NONE',  ( -1.592395536721566751, 0.1185427911281785041, 0.04121422034918794525 ) ) ;
#10321 = CARTESIAN_POINT ( 'NONE',  ( -0.06692913385815735250, -0.4881889763779528324, -0.5870514566507987197 ) ) ;
#10322 = EDGE_LOOP ( 'NONE', ( #2980, #12547, #257, #8804 ) ) ;
#10323 = VERTEX_POINT ( 'NONE', #8908 ) ;
#10324 = ORIENTED_EDGE ( 'NONE', *, *, #9143, .T. ) ;
#10325 = AXIS2_PLACEMENT_3D ( 'NONE', #2179, #15330, #764 ) ;
#10326 = AXIS2_PLACEMENT_3D ( 'NONE', #3670, #8444, #7792 ) ;
#10327 = DIRECTION ( 'NONE',  ( 0.000000000000000000, -0.000000000000000000, 1.000000000000000000 ) ) ;
#10328 = VECTOR ( 'NONE', #5361, 39.37007874015748143 ) ;
#10329 = AXIS2_PLACEMENT_3D ( 'NONE', #7015, #3731, #1373 ) ;
#10330 = FACE_OUTER_BOUND ( 'NONE', #9519, .T. ) ;
#10331 = FACE_OUTER_BOUND ( 'NONE', #2800, .T. ) ;
#10332 = DIRECTION ( 'NONE',  ( 0.000000000000000000, 0.000000000000000000, -1.000000000000000000 ) ) ;
#10333 = DIRECTION ( 'NONE',  ( 0.000000000000000000, 1.000000000000000000, 0.000000000000000000 ) ) ;
#10334 = ORIENTED_EDGE ( 'NONE', *, *, #4271, .F. ) ;
#10335 = DIRECTION ( 'NONE',  ( -0.000000000000000000, 1.000000000000000000, -0.000000000000000000 ) ) ;
#10336 = LINE ( 'NONE', #15126, #9100 ) ;
#10337 = CIRCLE ( 'NONE', #12111, 0.03937007874015751446 ) ;
#10338 = TOROIDAL_SURFACE ( 'NONE', #13844, 0.1614173228346456879, 0.003937007874015747977 ) ;
#10339 = CARTESIAN_POINT ( 'NONE',  ( 0.4552518684890383138, -0.09448818897637796532, 0.3855835468379170128 ) ) ;
#10340 = ADVANCED_FACE ( 'NONE', ( #5443 ), #14972, .F. ) ;
#10341 = DIRECTION ( 'NONE',  ( -0.8011800915434506010, 0.5984233124757325495, 0.000000000000000000 ) ) ;
#10342 = ORIENTED_EDGE ( 'NONE', *, *, #11099, .F. ) ;
#10343 = AXIS2_PLACEMENT_3D ( 'NONE', #12748, #10472, #7084 ) ;
#10344 = DIRECTION ( 'NONE',  ( -0.5000000000000004441, 0.000000000000000000, -0.8660254037844383745 ) ) ;
#10345 = AXIS2_PLACEMENT_3D ( 'NONE', #6212, #5189, #8566 ) ;
#10346 = ORIENTED_EDGE ( 'NONE', *, *, #5551, .T. ) ;
#10347 = EDGE_CURVE ( 'NONE', #15217, #14202, #11971, .T. ) ;
#10348 = DIMENSIONAL_EXPONENTS ( 1.000000000000000000, 0.000000000000000000, 0.000000000000000000, 0.000000000000000000, 0.000000000000000000, 0.000000000000000000, 0.000000000000000000 ) ;
#10349 = ORIENTED_EDGE ( 'NONE', *, *, #5832, .T. ) ;
#10350 = DIRECTION ( 'NONE',  ( 0.000000000000000000, -0.4999999999999979461, 0.8660254037844397068 ) ) ;
#10351 = CARTESIAN_POINT ( 'NONE',  ( -0.02641567992992046449, 0.1724028871747071145, 1.853431881210122409E-17 ) ) ;
#10352 = VECTOR ( 'NONE', #1133, 39.37007874015748143 ) ;
#10353 = AXIS2_PLACEMENT_3D ( 'NONE', #4093, #9909, #10133 ) ;
#10354 = AXIS2_PLACEMENT_3D ( 'NONE', #4154, #5009, #9808 ) ;
#10355 = DIRECTION ( 'NONE',  ( -0.5000000000000004441, -0.000000000000000000, -0.8660254037844384856 ) ) ;
#10356 = VECTOR ( 'NONE', #4627, 39.37007874015748143 ) ;
#10357 = CONTEXT_DEPENDENT_SHAPE_REPRESENTATION ( #9416, #6281 ) ;
#10358 = CARTESIAN_POINT ( 'NONE',  ( 0.05905511811029059283, -0.09842519685039370636, -0.2377126739437405434 ) ) ;
#10359 = CIRCLE ( 'NONE', #9865, 0.003937007874015749712 ) ;
#10360 = DIRECTION ( 'NONE',  ( -0.000000000000000000, -0.000000000000000000, -1.000000000000000000 ) ) ;
#10361 = EDGE_CURVE ( 'NONE', #9040, #14723, #8980, .T. ) ;
#10362 = VERTEX_POINT ( 'NONE', #1769 ) ;
#10363 = DIRECTION ( 'NONE',  ( -1.000000000000000000, 8.673617379884013384E-15, 0.000000000000000000 ) ) ;
#10364 = EDGE_CURVE ( 'NONE', #1922, #3058, #14780, .T. ) ;
#10365 = DIRECTION ( 'NONE',  ( 0.8660254037844389297, 0.000000000000000000, -0.4999999999999994449 ) ) ;
#10366 = CARTESIAN_POINT ( 'NONE',  ( -1.879669382776355979, -2.922326502959081029, -0.005509842852737917643 ) ) ;
#10367 = EDGE_CURVE ( 'NONE', #7381, #4497, #1459, .T. ) ;
#10368 = CARTESIAN_POINT ( 'NONE',  ( 0.000000000000000000, 0.03937007874015749365, 0.000000000000000000 ) ) ;
#10369 = CIRCLE ( 'NONE', #12121, 0.003937007874015724558 ) ;
#10370 = AXIS2_PLACEMENT_3D ( 'NONE', #1863, #6299, #11187 ) ;
#10371 = AXIS2_PLACEMENT_3D ( 'NONE', #10651, #2494, #7202 ) ;
#10372 = EDGE_LOOP ( 'NONE', ( #5936, #14241, #9188, #4073, #10060, #3859 ) ) ;
#10373 = EDGE_CURVE ( 'NONE', #1731, #11277, #8746, .T. ) ;
#10374 = LINE ( 'NONE', #11549, #13605 ) ;
#10375 = ORIENTED_EDGE ( 'NONE', *, *, #6616, .T. ) ;
#10376 = CIRCLE ( 'NONE', #3627, 0.03937007874015751446 ) ;
#10377 = VERTEX_POINT ( 'NONE', #11311 ) ;
#10378 = PRODUCT_DEFINITION_FORMATION_WITH_SPECIFIED_SOURCE ( 'ANY', '', #9801, .NOT_KNOWN. ) ;
#10379 = FACE_OUTER_BOUND ( 'NONE', #5322, .T. ) ;
#10380 = LINE ( 'NONE', #12575, #6065 ) ;
#10381 = LENGTH_MEASURE_WITH_UNIT ( LENGTH_MEASURE( 0.02539999999999999897 ), #912 );
#10382 = AXIS2_PLACEMENT_3D ( 'NONE', #12562, #572, #13811 ) ;
#10383 = VECTOR ( 'NONE', #9515, 39.37007874015748143 ) ;
#10384 = FACE_OUTER_BOUND ( 'NONE', #90, .T. ) ;
#10385 = EDGE_CURVE ( 'NONE', #15252, #9785, #2893, .T. ) ;
#10386 = DIRECTION ( 'NONE',  ( -0.5000000000000004441, 3.120833636094142350E-14, -0.8660254037844383745 ) ) ;
#10387 = CARTESIAN_POINT ( 'NONE',  ( 6.846450609406462919E-17, 1.417322834645669438, 0.5590551181102362266 ) ) ;
#10388 = CIRCLE ( 'NONE', #6882, 0.003937007874015724558 ) ;
#10389 = DIRECTION ( 'NONE',  ( 0.000000000000000000, 0.000000000000000000, 1.000000000000000000 ) ) ;
#10390 = EDGE_CURVE ( 'NONE', #14789, #986, #8455, .T. ) ;
#10391 = DIRECTION ( 'NONE',  ( 0.8144815189573203495, -0.5801894994542524664, -1.283760644411384396E-16 ) ) ;
#10392 = CARTESIAN_POINT ( 'NONE',  ( -2.100501784635051550, -1.630597114118274460, -0.1033464566929128137 ) ) ;
#10393 = VERTEX_POINT ( 'NONE', #7228 ) ;
#10394 = ADVANCED_FACE ( 'NONE', ( #10384 ), #2951, .T. ) ;
#10395 = ORIENTED_EDGE ( 'NONE', *, *, #3179, .F. ) ;
#10396 = AXIS2_PLACEMENT_3D ( 'NONE', #4598, #1247, #8135 ) ;
#10397 = ORIENTED_EDGE ( 'NONE', *, *, #8119, .T. ) ;
#10398 = CIRCLE ( 'NONE', #9660, 0.003937007874015749712 ) ;
#10399 = AXIS2_PLACEMENT_3D ( 'NONE', #566, #10132, #7615 ) ;
#10400 = VERTEX_POINT ( 'NONE', #12810 ) ;
#10401 = AXIS2_PLACEMENT_3D ( 'NONE', #1231, #13211, #13502 ) ;
#10402 = ADVANCED_FACE ( 'NONE', ( #9288 ), #8108, .F. ) ;
#10403 = CARTESIAN_POINT ( 'NONE',  ( -1.586197524890927024, 0.1268408028905886054, -0.05897664633272541035 ) ) ;
#10404 = CARTESIAN_POINT ( 'NONE',  ( -0.06692913385815731087, -0.2952755905511811330, -0.3797276218561366212 ) ) ;
#10405 = CARTESIAN_POINT ( 'NONE',  ( -0.08151194962748890827, 0.1637246173173402264, -0.03937007874015747977 ) ) ;
#10406 = CARTESIAN_POINT ( 'NONE',  ( -0.3441669734936866343, 2.010494531933507467, 0.03937007874015747977 ) ) ;
#10407 = VECTOR ( 'NONE', #10555, 39.37007874015748143 ) ;
#10408 = DIRECTION ( 'NONE',  ( 0.8660254037844431485, -4.956352788505159323E-16, 0.4999999999999918954 ) ) ;
#10409 = AXIS2_PLACEMENT_3D ( 'NONE', #12439, #6468, #7882 ) ;
#10410 = DIRECTION ( 'NONE',  ( 1.000000000000000000, 0.000000000000000000, 0.000000000000000000 ) ) ;
#10411 = CIRCLE ( 'NONE', #7653, 0.003937007874015758385 ) ;
#10412 = ORIENTED_EDGE ( 'NONE', *, *, #780, .F. ) ;
#10413 = DIRECTION ( 'NONE',  ( 1.224646799147353207E-16, 1.000000000000000000, 0.000000000000000000 ) ) ;
#10414 = DIRECTION ( 'NONE',  ( 0.000000000000000000, 0.000000000000000000, -1.000000000000000000 ) ) ;
#10415 = DIRECTION ( 'NONE',  ( 0.000000000000000000, 0.000000000000000000, 1.000000000000000000 ) ) ;
#10416 = TOROIDAL_SURFACE ( 'NONE', #7170, 0.7007874015748031260, 0.007874015748031495954 ) ;
#10417 = ORIENTED_EDGE ( 'NONE', *, *, #3505, .F. ) ;
#10418 = ORIENTED_EDGE ( 'NONE', *, *, #529, .T. ) ;
#10419 = EDGE_CURVE ( 'NONE', #11634, #8036, #13915, .T. ) ;
#10420 = EDGE_LOOP ( 'NONE', ( #10916, #845, #3522, #12925 ) ) ;
#10421 = CARTESIAN_POINT ( 'NONE',  ( 0.5905511811023620439, -0.003937007874015747977, 0.1591122789105293978 ) ) ;
#10422 = EDGE_CURVE ( 'NONE', #11956, #10983, #2202, .T. ) ;
#10423 = AXIS2_PLACEMENT_3D ( 'NONE', #12250, #13552, #9974 ) ;
#10424 = FACE_OUTER_BOUND ( 'NONE', #8740, .T. ) ;
#10425 = CARTESIAN_POINT ( 'NONE',  ( -1.970947046482191656, -2.817268671564700178, 0.1717492298712584298 ) ) ;
#10426 = CARTESIAN_POINT ( 'NONE',  ( 0.000000000000000000, 0.07874015748031495954, 0.000000000000000000 ) ) ;
#10427 = DIRECTION ( 'NONE',  ( -0.4999999999999998890, -5.810221930991196648E-16, 0.8660254037844387076 ) ) ;
#10428 = DIRECTION ( 'NONE',  ( -0.000000000000000000, -1.000000000000000000, 0.000000000000000000 ) ) ;
#10429 = ORIENTED_EDGE ( 'NONE', *, *, #10486, .T. ) ;
#10430 = DIRECTION ( 'NONE',  ( -0.000000000000000000, 1.000000000000000000, 0.000000000000000000 ) ) ;
#10431 = DIRECTION ( 'NONE',  ( 0.000000000000000000, 1.000000000000000000, 0.000000000000000000 ) ) ;
#10432 = AXIS2_PLACEMENT_3D ( 'NONE', #13419, #9818, #6197 ) ;
#10433 = CARTESIAN_POINT ( 'NONE',  ( 0.4591888763630541104, -0.4921259842519685179, 0.3787644491703230365 ) ) ;
#10434 = CARTESIAN_POINT ( 'NONE',  ( -0.03346456692910660530, -0.4881889763779528324, -0.05796233017450189845 ) ) ;
#10435 = ORIENTED_EDGE ( 'NONE', *, *, #2774, .F. ) ;
#10436 = CARTESIAN_POINT ( 'NONE',  ( 0.1181102362204724532, 2.637795275590551825, 0.03937007874015747977 ) ) ;
#10437 = VECTOR ( 'NONE', #10254, 39.37007874015748143 ) ;
#10438 = ORIENTED_EDGE ( 'NONE', *, *, #14895, .T. ) ;
#10439 = ORIENTED_EDGE ( 'NONE', *, *, #6170, .F. ) ;
#10440 = AXIS2_PLACEMENT_3D ( 'NONE', #14424, #3528, #10659 ) ;
#10441 = CARTESIAN_POINT ( 'NONE',  ( -0.09842519685028340570, -0.4921259842519685179, -0.5870514566507987197 ) ) ;
#10442 = CARTESIAN_POINT ( 'NONE',  ( 0.4854723491485768982, 1.043307086614173373, 0.3484785681409844904 ) ) ;
#10443 = CIRCLE ( 'NONE', #1931, 0.003937007874015758385 ) ;
#10444 = CARTESIAN_POINT ( 'NONE',  ( -0.4552518684890389244, -0.09842519685039370636, 0.3855835468379172903 ) ) ;
#10445 = FACE_OUTER_BOUND ( 'NONE', #4460, .T. ) ;
#10446 = CIRCLE ( 'NONE', #2694, 0.7007874015748031260 ) ;
#10447 = DIRECTION ( 'NONE',  ( 0.8660254037844387076, 0.000000000000000000, 0.4999999999999996669 ) ) ;
#10448 = ORIENTED_EDGE ( 'NONE', *, *, #4, .F. ) ;
#10449 = CARTESIAN_POINT ( 'NONE',  ( 0.000000000000000000, -0.4881889763779528324, 0.000000000000000000 ) ) ;
#10450 = CARTESIAN_POINT ( 'NONE',  ( 0.2647411304680618027, -0.4921259842519685179, 0.03404161279868787859 ) ) ;
#10451 = CIRCLE ( 'NONE', #12457, 0.003937007874015724558 ) ;
#10452 = DIRECTION ( 'NONE',  ( 0.4999999999999976130, -0.000000000000000000, 0.8660254037844400399 ) ) ;
#10453 = FILL_AREA_STYLE_COLOUR ( '', #13704 ) ;
#10454 = ORIENTED_EDGE ( 'NONE', *, *, #4601, .T. ) ;
#10455 = ORIENTED_EDGE ( 'NONE', *, *, #7586, .F. ) ;
#10456 = CARTESIAN_POINT ( 'NONE',  ( -0.2362204724409448231, -0.02638708502139245488, 0.03937007874015747977 ) ) ;
#10457 = ORIENTED_EDGE ( 'NONE', *, *, #10029, .F. ) ;
#10458 = TOROIDAL_SURFACE ( 'NONE', #3214, 0.5984251968503937480, 0.007874015748031495954 ) ;
#10459 = EDGE_LOOP ( 'NONE', ( #6705, #3480, #8452, #4546, #7573 ) ) ;
#10460 = EDGE_CURVE ( 'NONE', #7381, #14663, #7448, .T. ) ;
#10461 = ORIENTED_EDGE ( 'NONE', *, *, #7915, .T. ) ;
#10462 = CARTESIAN_POINT ( 'NONE',  ( -2.755905511811024056, -2.772329397582842248, 0.000000000000000000 ) ) ;
#10463 = EDGE_CURVE ( 'NONE', #11432, #6409, #7947, .T. ) ;
#10464 = DIRECTION ( 'NONE',  ( 0.000000000000000000, -1.000000000000000000, -0.000000000000000000 ) ) ;
#10465 = DIRECTION ( 'NONE',  ( 0.5000000000000001110, -0.000000000000000000, -0.8660254037844385966 ) ) ;
#10466 = AXIS2_PLACEMENT_3D ( 'NONE', #10035, #6253, #2586 ) ;
#10467 = CARTESIAN_POINT ( 'NONE',  ( 0.4330708661417309036, -0.09448818897637796532, 0.4318761856142889766 ) ) ;
#10468 = LINE ( 'NONE', #4580, #8154 ) ;
#10469 = ADVANCED_FACE ( 'NONE', ( #3326 ), #11556, .F. ) ;
#10470 = CARTESIAN_POINT ( 'NONE',  ( -1.389958893394353412, -0.02151193858058574049, 0.06001963939216824889 ) ) ;
#10471 = CIRCLE ( 'NONE', #4949, 0.1279527559055117780 ) ;
#10472 = DIRECTION ( 'NONE',  ( 0.000000000000000000, -1.000000000000000000, 0.000000000000000000 ) ) ;
#10473 = DIRECTION ( 'NONE',  ( 0.000000000000000000, 0.000000000000000000, -1.000000000000000000 ) ) ;
#10474 = ORIENTED_EDGE ( 'NONE', *, *, #4265, .F. ) ;
#10475 = ORIENTED_EDGE ( 'NONE', *, *, #10262, .T. ) ;
#10476 = AXIS2_PLACEMENT_3D ( 'NONE', #3687, #8464, #11685 ) ;
#10477 = ORIENTED_EDGE ( 'NONE', *, *, #2906, .F. ) ;
#10478 = VERTEX_POINT ( 'NONE', #5585 ) ;
#10479 = ADVANCED_FACE ( 'NONE', ( #4504 ), #7956, .T. ) ;
#10480 = EDGE_CURVE ( 'NONE', #11872, #5535, #13461, .T. ) ;
#10481 = DIRECTION ( 'NONE',  ( 0.000000000000000000, 0.000000000000000000, 1.000000000000000000 ) ) ;
#10482 = CARTESIAN_POINT ( 'NONE',  ( -0.02636306718619302325, 0.1724112960300248354, 0.0009221601458071186511 ) ) ;
#10483 = CARTESIAN_POINT ( 'NONE',  ( 1.928577636452524610E-17, 0.03149606299212599769, 0.1574803149606299191 ) ) ;
#10484 = EDGE_CURVE ( 'NONE', #1810, #3677, #3944, .T. ) ;
#10485 = DIRECTION ( 'NONE',  ( 0.000000000000000000, 0.000000000000000000, -1.000000000000000000 ) ) ;
#10486 = EDGE_CURVE ( 'NONE', #8145, #5520, #14713, .T. ) ;
#10487 = CARTESIAN_POINT ( 'NONE',  ( -1.141732283464566677, 4.821444091131322309E-18, -0.02559055118110236185 ) ) ;
#10488 = DIRECTION ( 'NONE',  ( 0.000000000000000000, 0.000000000000000000, -1.000000000000000000 ) ) ;
#10489 = EDGE_LOOP ( 'NONE', ( #6087, #12427 ) ) ;
#10490 = DIRECTION ( 'NONE',  ( -0.000000000000000000, 1.000000000000000000, -0.000000000000000000 ) ) ;
#10491 = CARTESIAN_POINT ( 'NONE',  ( 0.05114323250695499562, 0.000000000000000000, -0.08858267716535433989 ) ) ;
#10492 = ORIENTED_EDGE ( 'NONE', *, *, #14541, .F. ) ;
#10493 = ORIENTED_EDGE ( 'NONE', *, *, #11729, .F. ) ;
#10494 = ORIENTED_EDGE ( 'NONE', *, *, #7425, .T. ) ;
#10495 = DIRECTION ( 'NONE',  ( -0.000000000000000000, -1.000000000000000000, -0.000000000000000000 ) ) ;
#10496 = CARTESIAN_POINT ( 'NONE',  ( 0.4296613173079339432, -0.09448818897637796532, 0.4299076816772811060 ) ) ;
#10497 = CARTESIAN_POINT ( 'NONE',  ( -1.931857757055364777, -2.930757773757384665, 0.08017971412056627833 ) ) ;
#10498 = EDGE_CURVE ( 'NONE', #10242, #4029, #14150, .T. ) ;
#10499 = LINE ( 'NONE', #14653, #7932 ) ;
#10500 = FACE_OUTER_BOUND ( 'NONE', #8995, .T. ) ;
#10501 = VERTEX_POINT ( 'NONE', #3257 ) ;
#10502 =( REPRESENTATION_RELATIONSHIP ('NONE','NONE', #8904, #6262 ) REPRESENTATION_RELATIONSHIP_WITH_TRANSFORMATION ( #886 )SHAPE_REPRESENTATION_RELATIONSHIP( ) );
#10503 = DIRECTION ( 'NONE',  ( 0.8660254037844383745, 0.000000000000000000, -0.5000000000000004441 ) ) ;
#10504 = CARTESIAN_POINT ( 'NONE',  ( -0.5445274672588088505, 1.338626482899105241, 0.2461921031270815630 ) ) ;
#10505 = CARTESIAN_POINT ( 'NONE',  ( -0.07874015748031501505, 0.1442356988431297560, 0.05905511811023622659 ) ) ;
#10506 = LINE ( 'NONE', #5784, #6571 ) ;
#10507 = ORIENTED_EDGE ( 'NONE', *, *, #14722, .T. ) ;
#10508 = ADVANCED_FACE ( 'NONE', ( #4430 ), #13953, .T. ) ;
#10509 = DIRECTION ( 'NONE',  ( -0.8660254037844405950, 0.000000000000000000, 0.4999999999999966693 ) ) ;
#10510 = EDGE_LOOP ( 'NONE', ( #7302, #8790, #7541, #9715 ) ) ;
#10511 = ORIENTED_EDGE ( 'NONE', *, *, #13815, .F. ) ;
#10512 = ORIENTED_EDGE ( 'NONE', *, *, #7321, .T. ) ;
#10513 = VERTEX_POINT ( 'NONE', #996 ) ;
#10514 = CARTESIAN_POINT ( 'NONE',  ( 0.000000000000000000, 0.003937007874015749712, 0.000000000000000000 ) ) ;
#10515 = CARTESIAN_POINT ( 'NONE',  ( -0.005352459137615327503, 0.1648200595001707847, 1.247430111210527045E-16 ) ) ;
#10516 = DIRECTION ( 'NONE',  ( -0.8660254037844383745, 0.000000000000000000, 0.5000000000000004441 ) ) ;
#10517 = DIRECTION ( 'NONE',  ( 0.000000000000000000, 0.000000000000000000, -1.000000000000000000 ) ) ;
#10518 = CONTEXT_DEPENDENT_SHAPE_REPRESENTATION ( #11811, #12316 ) ;
#10519 = CARTESIAN_POINT ( 'NONE',  ( -1.100415514366371639, -0.04998955061625907220, 0.03937007874015747977 ) ) ;
#10520 = CARTESIAN_POINT ( 'NONE',  ( -0.07022707542947256854, -0.1870727099175781838, 0.03937007874015747283 ) ) ;
#10521 = ORIENTED_EDGE ( 'NONE', *, *, #1301, .F. ) ;
#10522 = CARTESIAN_POINT ( 'NONE',  ( -1.969722513608740178, -2.871257544293922770, -0.1475413299907661346 ) ) ;
#10523 = DIRECTION ( 'NONE',  ( -0.000000000000000000, 1.000000000000000000, -0.000000000000000000 ) ) ;
#10524 = DIRECTION ( 'NONE',  ( -0.8660254037844383745, 0.000000000000000000, -0.5000000000000004441 ) ) ;
#10525 = CARTESIAN_POINT ( 'NONE',  ( -0.5452755905511542656, -0.4881889763779528324, 0.2375319020879049503 ) ) ;
#10526 = DIRECTION ( 'NONE',  ( 0.000000000000000000, 0.000000000000000000, -1.000000000000000000 ) ) ;
#10527 = EDGE_CURVE ( 'NONE', #776, #13544, #458, .T. ) ;
#10528 = PRESENTATION_STYLE_ASSIGNMENT (( #896 ) ) ;
#10529 = ORIENTED_EDGE ( 'NONE', *, *, #15243, .T. ) ;
#10530 = ORIENTED_EDGE ( 'NONE', *, *, #7705, .F. ) ;
#10531 = PLANE ( 'NONE',  #3182 ) ;
#10532 = EDGE_LOOP ( 'NONE', ( #3922, #3660 ) ) ;
#10533 = ORIENTED_EDGE ( 'NONE', *, *, #15461, .F. ) ;
#10534 = VERTEX_POINT ( 'NONE', #13992 ) ;
#10535 = CARTESIAN_POINT ( 'NONE',  ( -2.080881322745466999, -1.632190302820504479, 0.08366141732283424726 ) ) ;
#10536 = DIRECTION ( 'NONE',  ( -0.8660254037844400399, -5.421010862427505407E-16, 0.4999999999999976130 ) ) ;
#10537 = CARTESIAN_POINT ( 'NONE',  ( -1.897981793197825340, -2.949207328992450083, -0.01172296963439428338 ) ) ;
#10538 = FACE_OUTER_BOUND ( 'NONE', #4551, .T. ) ;
#10539 = CARTESIAN_POINT ( 'NONE',  ( 0.4307978335858662633, -0.09448818897637796532, 0.4279391777402732910 ) ) ;
#10540 = DIRECTION ( 'NONE',  ( 0.8660254037844383745, -9.486769009248228879E-16, -0.5000000000000004441 ) ) ;
#10541 = CARTESIAN_POINT ( 'NONE',  ( -0.1618514667033796040, -0.4881889763779528324, 0.2083147301385909200 ) ) ;
#10542 = LINE ( 'NONE', #15170, #4358 ) ;
#10543 = ADVANCED_FACE ( 'NONE', ( #8028 ), #413, .T. ) ;
#10544 = DIRECTION ( 'NONE',  ( 0.000000000000000000, -0.000000000000000000, 1.000000000000000000 ) ) ;
#10545 = EDGE_CURVE ( 'NONE', #11243, #9720, #2447, .T. ) ;
#10546 = ORIENTED_EDGE ( 'NONE', *, *, #7027, .F. ) ;
#10547 = ORIENTED_EDGE ( 'NONE', *, *, #5653, .T. ) ;
#10548 = ORIENTED_EDGE ( 'NONE', *, *, #4247, .T. ) ;
#10549 = EDGE_LOOP ( 'NONE', ( #2249, #14707, #761, #13631 ) ) ;
#10550 = ADVANCED_FACE ( 'NONE', ( #192 ), #1504, .T. ) ;
#10551 = DIRECTION ( 'NONE',  ( 0.8660254037844365982, -0.000000000000000000, 0.5000000000000035527 ) ) ;
#10552 = CARTESIAN_POINT ( 'NONE',  ( -0.01753362615437764269, 0.1513390073937369296, 0.03062283071528665995 ) ) ;
#10553 = FACE_OUTER_BOUND ( 'NONE', #4044, .T. ) ;
#10554 = CARTESIAN_POINT ( 'NONE',  ( -0.04921259842516954863, -0.4881889763779528324, -0.08523872084487790768 ) ) ;
#10555 = DIRECTION ( 'NONE',  ( -0.000000000000000000, -1.000000000000000000, -0.000000000000000000 ) ) ;
#10556 = ORIENTED_EDGE ( 'NONE', *, *, #9901, .T. ) ;
#10557 = DIRECTION ( 'NONE',  ( -0.000000000000000000, -0.000000000000000000, -1.000000000000000000 ) ) ;
#10558 = LINE ( 'NONE', #11820, #7638 ) ;
#10559 = EDGE_CURVE ( 'NONE', #2689, #12058, #3843, .T. ) ;
#10560 = DIMENSIONAL_EXPONENTS ( 1.000000000000000000, 0.000000000000000000, 0.000000000000000000, 0.000000000000000000, 0.000000000000000000, 0.000000000000000000, 0.000000000000000000 ) ;
#10561 = ADVANCED_FACE ( 'NONE', ( #11126 ), #326, .F. ) ;
#10562 = EDGE_LOOP ( 'NONE', ( #13067, #2352, #12852, #9311 ) ) ;
#10563 = ORIENTED_EDGE ( 'NONE', *, *, #13057, .T. ) ;
#10564 = EDGE_CURVE ( 'NONE', #6005, #2150, #8708, .T. ) ;
#10565 = ORIENTED_EDGE ( 'NONE', *, *, #10765, .F. ) ;
#10566 = DIRECTION ( 'NONE',  ( -1.000000000000000000, 0.000000000000000000, 0.000000000000000000 ) ) ;
#10567 = DIRECTION ( 'NONE',  ( -0.000000000000000000, -1.000000000000000000, -0.000000000000000000 ) ) ;
#10568 = CARTESIAN_POINT ( 'NONE',  ( -1.938704201247565928, -2.911695145306065324, -0.1100133229241002375 ) ) ;
#10569 = CYLINDRICAL_SURFACE ( 'NONE', #5428, 0.003937007874015721089 ) ;
#10570 = CYLINDRICAL_SURFACE ( 'NONE', #10440, 0.003937007874015741038 ) ;
#10571 = CARTESIAN_POINT ( 'NONE',  ( -1.938022636209871363, -2.767800838503367888, 0.1776221991034347969 ) ) ;
#10572 = ORIENTED_EDGE ( 'NONE', *, *, #8096, .F. ) ;
#10573 = LINE ( 'NONE', #2034, #5160 ) ;
#10574 = FACE_OUTER_BOUND ( 'NONE', #6720, .T. ) ;
#10575 = PLANE ( 'NONE',  #4202 ) ;
#10576 = EDGE_CURVE ( 'NONE', #3335, #11465, #5191, .T. ) ;
#10577 = CARTESIAN_POINT ( 'NONE',  ( 0.4552518684890383138, -0.09842519685039370636, 0.3855835468379170128 ) ) ;
#10578 = ORIENTED_EDGE ( 'NONE', *, *, #1538, .T. ) ;
#10579 = DIRECTION ( 'NONE',  ( 1.000000000000000000, 0.000000000000000000, 0.000000000000000000 ) ) ;
#10580 = VECTOR ( 'NONE', #13059, 39.37007874015748143 ) ;
#10581 = ORIENTED_EDGE ( 'NONE', *, *, #1370, .F. ) ;
#10582 = AXIS2_PLACEMENT_3D ( 'NONE', #14549, #8516, #13457 ) ;
#10583 = EDGE_CURVE ( 'NONE', #5216, #8739, #13218, .T. ) ;
#10584 = AXIS2_PLACEMENT_3D ( 'NONE', #6135, #9598, #7173 ) ;
#10585 = EDGE_CURVE ( 'NONE', #5700, #9905, #3776, .T. ) ;
#10586 = VERTEX_POINT ( 'NONE', #14513 ) ;
#10587 =( BOUNDED_CURVE ( )  B_SPLINE_CURVE ( 3, ( #3312, #6753, #14283, #12874 ),
 .UNSPECIFIED., .F., .T. ) 
 B_SPLINE_CURVE_WITH_KNOTS ( ( 4, 4 ),
 ( 1.570796326794896558, 3.141592653589793116 ),
 .UNSPECIFIED. ) 
 CURVE ( )  GEOMETRIC_REPRESENTATION_ITEM ( )  RATIONAL_B_SPLINE_CURVE ( ( 1.000000000000000000, 0.8047378541243649375, 0.8047378541243649375, 1.000000000000000000 ) ) 
 REPRESENTATION_ITEM ( '' )  );
#10588 = CARTESIAN_POINT ( 'NONE',  ( -0.4625984251968516259, -0.09842519685039370636, 0.3807329531073311846 ) ) ;
#10589 = DIRECTION ( 'NONE',  ( 0.4999999999999966693, 0.000000000000000000, 0.8660254037844405950 ) ) ;
#10590 = EDGE_CURVE ( 'NONE', #12965, #8519, #15220, .T. ) ;
#10591 = CARTESIAN_POINT ( 'NONE',  ( -1.599593005878032992, 0.1086758623451425237, -0.04860704773263154616 ) ) ;
#10592 = CARTESIAN_POINT ( 'NONE',  ( -2.755905511811024056, -2.772329397582842248, -0.1771653543307079026 ) ) ;
#10593 = FACE_OUTER_BOUND ( 'NONE', #5767, .T. ) ;
#10594 = VECTOR ( 'NONE', #9297, 39.37007874015748143 ) ;
#10595 = CIRCLE ( 'NONE', #9343, 0.04330708661417329020 ) ;
#10596 = DIRECTION ( 'NONE',  ( -1.000000000000000000, 0.000000000000000000, 0.000000000000000000 ) ) ;
#10597 = ORIENTED_EDGE ( 'NONE', *, *, #1426, .T. ) ;
#10598 = CARTESIAN_POINT ( 'NONE',  ( 0.06767366483286080259, -0.2952755905511811330, 0.7209811753676967916 ) ) ;
#10599 = CIRCLE ( 'NONE', #1334, 0.007874015748031499423 ) ;
#10600 = AXIS2_PLACEMENT_3D ( 'NONE', #10270, #7831, #789 ) ;
#10601 = DIRECTION ( 'NONE',  ( -0.8660254037844385966, 0.000000000000000000, -0.5000000000000000000 ) ) ;
#10602 = CARTESIAN_POINT ( 'NONE',  ( 0.5379290338433416752, -0.1023622047244094474, 0.2423824958184916112 ) ) ;
#10603 = VERTEX_POINT ( 'NONE', #7590 ) ;
#10604 = CARTESIAN_POINT ( 'NONE',  ( -0.1022864650139100884, 0.05905511811023622659, -1.048351444896847144E-20 ) ) ;
#10606 = ORIENTED_EDGE ( 'NONE', *, *, #8930, .T. ) ;
#10605 = CIRCLE ( 'NONE', #10843, 1.885039370078740451 ) ;
#10607 = AXIS2_PLACEMENT_3D ( 'NONE', #4556, #10355, #10516 ) ;
#10608 = ORIENTED_EDGE ( 'NONE', *, *, #11755, .T. ) ;
#10609 = CIRCLE ( 'NONE', #10103, 0.5511811023622046335 ) ;
#10610 = ORIENTED_EDGE ( 'NONE', *, *, #3095, .F. ) ;
#10611 = CARTESIAN_POINT ( 'NONE',  ( 0.5418660417173575272, -0.4881889763779528324, 0.2355633981508976349 ) ) ;
#10612 = EDGE_CURVE ( 'NONE', #4737, #11240, #12472, .T. ) ;
#10613 = CARTESIAN_POINT ( 'NONE',  ( 0.000000000000000000, 2.165354330708661568, 0.000000000000000000 ) ) ;
#10614 = CARTESIAN_POINT ( 'NONE',  ( -1.950289002586781173, -2.794939870759669098, 0.1760869912453440211 ) ) ;
#10615 = CARTESIAN_POINT ( 'NONE',  ( -1.365923996832131609E-16, 36.18795473304007970, 6.829619984160658046E-17 ) ) ;
#10616 = CARTESIAN_POINT ( 'NONE',  ( -1.957251767100264495, -2.772329397581817734, -0.1771653543307079026 ) ) ;
#10617 = DIRECTION ( 'NONE',  ( -0.4999999999999995004, -0.000000000000000000, -0.8660254037844390407 ) ) ;
#10618 = DIRECTION ( 'NONE',  ( -0.5000000000000000000, 0.000000000000000000, 0.8660254037844385966 ) ) ;
#10619 = DIRECTION ( 'NONE',  ( -0.000000000000000000, -1.000000000000000000, -0.000000000000000000 ) ) ;
#10620 = AXIS2_PLACEMENT_3D ( 'NONE', #3820, #2883, #1639 ) ;
#10621 = CIRCLE ( 'NONE', #11110, 0.003937007874015741038 ) ;
#10622 = VECTOR ( 'NONE', #1322, 39.37007874015748143 ) ;
#10623 = DIRECTION ( 'NONE',  ( 1.000000000000000000, 0.000000000000000000, 0.000000000000000000 ) ) ;
#10624 = DIRECTION ( 'NONE',  ( 0.4999999999999981681, 0.000000000000000000, 0.8660254037844397068 ) ) ;
#10625 = CIRCLE ( 'NONE', #7100, 0.003937007874015737569 ) ;
#10626 = AXIS2_PLACEMENT_3D ( 'NONE', #3307, #11614, #4785 ) ;
#10627 = EDGE_LOOP ( 'NONE', ( #7055, #13955 ) ) ;
#10628 = AXIS2_PLACEMENT_3D ( 'NONE', #14462, #8499, #10834 ) ;
#10629 = ORIENTED_EDGE ( 'NONE', *, *, #11002, .T. ) ;
#10630 = ORIENTED_EDGE ( 'NONE', *, *, #14807, .T. ) ;
#10631 = ORIENTED_EDGE ( 'NONE', *, *, #12054, .F. ) ;
#10632 = VECTOR ( 'NONE', #4096, 39.37007874015748143 ) ;
#10633 = AXIS2_PLACEMENT_3D ( 'NONE', #1439, #14583, #12022 ) ;
#10634 = VECTOR ( 'NONE', #4720, 39.37007874015748143 ) ;
#10635 = CARTESIAN_POINT ( 'NONE',  ( -1.107198012490790306, -0.06846922848666045502, 0.05905511811023622659 ) ) ;
#10636 = CIRCLE ( 'NONE', #9891, 0.003937007874015758385 ) ;
#10637 = CYLINDRICAL_SURFACE ( 'NONE', #1447, 0.7086614173228346081 ) ;
#10638 = DIRECTION ( 'NONE',  ( -0.000000000000000000, 0.000000000000000000, 1.000000000000000000 ) ) ;
#10639 = DIRECTION ( 'NONE',  ( -1.224646799147353947E-16, 0.000000000000000000, -1.000000000000000000 ) ) ;
#10640 = ORIENTED_EDGE ( 'NONE', *, *, #8820, .F. ) ;
#10641 = CARTESIAN_POINT ( 'NONE',  ( 0.000000000000000000, 0.000000000000000000, 0.000000000000000000 ) ) ;
#10642 = ADVANCED_FACE ( 'NONE', ( #5011 ), #4008, .T. ) ;
#10643 = CARTESIAN_POINT ( 'NONE',  ( 0.05114323250695503031, 0.05905511811023622659, 0.08858267716535433989 ) ) ;
#10644 = CIRCLE ( 'NONE', #14408, 0.003937007874015754916 ) ;
#10645 = VECTOR ( 'NONE', #3632, 39.37007874015748143 ) ;
#10646 = AXIS2_PLACEMENT_3D ( 'NONE', #8557, #8726, #6205 ) ;
#10647 = ORIENTED_EDGE ( 'NONE', *, *, #8854, .F. ) ;
#10648 = ORIENTED_EDGE ( 'NONE', *, *, #4848, .F. ) ;
#10649 = AXIS2_PLACEMENT_3D ( 'NONE', #3122, #391, #9954 ) ;
#10650 = ORIENTED_EDGE ( 'NONE', *, *, #1484, .T. ) ;
#10651 = CARTESIAN_POINT ( 'NONE',  ( 0.000000000000000000, -0.4881889763779528324, 0.000000000000000000 ) ) ;
#10652 = VECTOR ( 'NONE', #1396, 39.37007874015748854 ) ;
#10653 = CIRCLE ( 'NONE', #5640, 0.04330708661417331101 ) ;
#10654 = EDGE_CURVE ( 'NONE', #11417, #13359, #8978, .T. ) ;
#10655 = CIRCLE ( 'NONE', #4892, 0.003937007874015750579 ) ;
#10656 = LINE ( 'NONE', #4616, #2359 ) ;
#10657 = CARTESIAN_POINT ( 'NONE',  ( 0.1629063847838169432, -0.1023622047244094474, 0.2122517380126066888 ) ) ;
#10658 = LINE ( 'NONE', #4618, #2939 ) ;
#10659 = DIRECTION ( 'NONE',  ( -1.000000000000000000, 0.000000000000000000, -3.476578583725183758E-16 ) ) ;
#10660 = AXIS2_PLACEMENT_3D ( 'NONE', #4912, #10857, #293 ) ;
#10661 = CARTESIAN_POINT ( 'NONE',  ( -1.929649418975808439, -2.791725965709412449, 0.1763356003537114580 ) ) ;
#10662 = EDGE_LOOP ( 'NONE', ( #6411, #3351 ) ) ;
#10663 = DIRECTION ( 'NONE',  ( -0.3150766955165275607, 0.9411644975924603473, 0.1222131924708513701 ) ) ;
#10664 = B_SPLINE_CURVE_WITH_KNOTS ( 'NONE', 3,
 ( #4829, #9628, #14406, #6068 ),
 .UNSPECIFIED., .F., .F.,
 ( 4, 4 ),
 ( 0.000000000000000000, 0.002383301291214095802 ),
 .UNSPECIFIED. ) ;
#10665 = EDGE_CURVE ( 'NONE', #6873, #10081, #3714, .T. ) ;
#10666 = CARTESIAN_POINT ( 'NONE',  ( 0.3964138223131414840, -0.2952755905511811330, 0.1515865201236449578 ) ) ;
#10667 = CARTESIAN_POINT ( 'NONE',  ( -1.293236445124221312, 0.1355266887446167634, 0.03937007874015747977 ) ) ;
#10668 = DIRECTION ( 'NONE',  ( 1.000000000000000000, -8.673617379884051249E-15, -7.523163845262650140E-29 ) ) ;
#10669 = ORIENTED_EDGE ( 'NONE', *, *, #2711, .F. ) ;
#10670 = CIRCLE ( 'NONE', #2411, 0.003937007874015750579 ) ;
#10671 = ORIENTED_EDGE ( 'NONE', *, *, #4908, .T. ) ;
#10672 = ORIENTED_EDGE ( 'NONE', *, *, #12573, .T. ) ;
#10673 = DIMENSIONAL_EXPONENTS ( 1.000000000000000000, 0.000000000000000000, 0.000000000000000000, 0.000000000000000000, 0.000000000000000000, 0.000000000000000000, 0.000000000000000000 ) ;
#10674 = EDGE_LOOP ( 'NONE', ( #2380, #5971, #5003, #14002 ) ) ;
#10675 = VECTOR ( 'NONE', #1918, 39.37007874015748143 ) ;
#10676 = EDGE_CURVE ( 'NONE', #2543, #13376, #7685, .T. ) ;
#10677 = LINE ( 'NONE', #10808, #8082 ) ;
#10678 = CYLINDRICAL_SURFACE ( 'NONE', #1904, 0.003937007874015724558 ) ;
#10679 = ADVANCED_FACE ( 'NONE', ( #7452 ), #6446, .F. ) ;
#10680 = CARTESIAN_POINT ( 'NONE',  ( -1.598024100230236444, 0.1108858885491604135, -0.04651107584905353476 ) ) ;
#10681 = ITEM_DEFINED_TRANSFORMATION ( 'NONE', 'NONE', #6096,  #11481 ) ;
#10682 = DIRECTION ( 'NONE',  ( 1.000000000000000000, 0.000000000000000000, -9.159339953157533381E-13 ) ) ;
#10683 = AXIS2_PLACEMENT_3D ( 'NONE', #7298, #201, #9752 ) ;
#10684 = LINE ( 'NONE', #3628, #3370 ) ;
#10685 = ORIENTED_EDGE ( 'NONE', *, *, #1076, .T. ) ;
#10686 = DIRECTION ( 'NONE',  ( 0.000000000000000000, -0.000000000000000000, 1.000000000000000000 ) ) ;
#10687 = EDGE_CURVE ( 'NONE', #7239, #2402, #9967, .T. ) ;
#10688 = EDGE_CURVE ( 'NONE', #2574, #105, #6964, .T. ) ;
#10689 = DIRECTION ( 'NONE',  ( -0.000000000000000000, 1.000000000000000000, 0.000000000000000000 ) ) ;
#10690 = CIRCLE ( 'NONE', #12430, 0.04330708661417324162 ) ;
#10691 = CARTESIAN_POINT ( 'NONE',  ( 0.4591888763630541104, -0.4881889763779528324, 0.3787644491703230365 ) ) ;
#10692 = ORIENTED_EDGE ( 'NONE', *, *, #12770, .F. ) ;
#10693 = ORIENTED_EDGE ( 'NONE', *, *, #9517, .F. ) ;
#10694 = TOROIDAL_SURFACE ( 'NONE', #10197, 0.05905511811023614333, 0.01968503937007873988 ) ;
#10695 = ORIENTED_EDGE ( 'NONE', *, *, #2809, .F. ) ;
#10696 = EDGE_LOOP ( 'NONE', ( #12750, #12505, #815, #2006 ) ) ;
#10697 = AXIS2_PLACEMENT_3D ( 'NONE', #8938, #1795, #10183 ) ;
#10698 = LINE ( 'NONE', #14371, #11869 ) ;
#10699 = CARTESIAN_POINT ( 'NONE',  ( 0.1609378808468091004, -0.1023622047244094474, 0.2156612868464037047 ) ) ;
#10700 = CIRCLE ( 'NONE', #5680, 0.007874015748031449116 ) ;
#10701 = CARTESIAN_POINT ( 'NONE',  ( 0.4121618538092042261, -0.2952755905511811330, 0.1243101294532688583 ) ) ;
#10702 = DIRECTION ( 'NONE',  ( 0.000000000000000000, 0.000000000000000000, 1.000000000000000000 ) ) ;
#10703 = ADVANCED_FACE ( 'NONE', ( #14982 ), #3056, .T. ) ;
#10704 = AXIS2_PLACEMENT_3D ( 'NONE', #13365, #6151, #10941 ) ;
#10705 = CARTESIAN_POINT ( 'NONE',  ( -0.03886060139087894189, 0.06736074103232447818, -0.08219815605944147396 ) ) ;
#10706 = CARTESIAN_POINT ( 'NONE',  ( 0.06299212598430634080, -0.2952755905511811885, -0.3757906139821208247 ) ) ;
#10707 = ADVANCED_FACE ( 'NONE', ( #3223, #2031 ), #5401, .F. ) ;
#10708 = ORIENTED_EDGE ( 'NONE', *, *, #3219, .F. ) ;
#10709 = ADVANCED_FACE ( 'NONE', ( #14905 ), #7827, .T. ) ;
#10710 = ORIENTED_EDGE ( 'NONE', *, *, #1760, .F. ) ;
#10711 = ORIENTED_EDGE ( 'NONE', *, *, #10075, .T. ) ;
#10712 = VERTEX_POINT ( 'NONE', #12708 ) ;
#10713 = AXIS2_PLACEMENT_3D ( 'NONE', #8381, #1101, #5857 ) ;
#10714 = CARTESIAN_POINT ( 'NONE',  ( -0.7455328141524870667, 1.338582677165354395, 0.3622425942647020669 ) ) ;
#10715 = CIRCLE ( 'NONE', #961, 0.003937007874015750579 ) ;
#10716 = CARTESIAN_POINT ( 'NONE',  ( 1.137795275590550936, 4.097147066950659020E-16, -0.02559055118110236185 ) ) ;
#10717 = LINE ( 'NONE', #9705, #10889 ) ;
#10718 = FACE_OUTER_BOUND ( 'NONE', #3855, .T. ) ;
#10719 = DIRECTION ( 'NONE',  ( 0.5000000000000001110, 0.000000000000000000, -0.8660254037844385966 ) ) ;
#10720 = EDGE_LOOP ( 'NONE', ( #1141, #11260, #3333, #14165 ) ) ;
#10721 = CARTESIAN_POINT ( 'NONE',  ( -1.452763252956527751, -0.05091287232363173737, 0.1033464566929133133 ) ) ;
#10722 = FACE_BOUND ( 'NONE', #9091, .T. ) ;
#10723 = DIRECTION ( 'NONE',  ( -0.8180917953313905366, 0.5750876580239416835, 0.000000000000000000 ) ) ;
#10724 = AXIS2_PLACEMENT_3D ( 'NONE', #769, #3206, #622 ) ;
#10725 = VERTEX_POINT ( 'NONE', #1891 ) ;
#10726 = ADVANCED_FACE ( 'NONE', ( #6651 ), #8952, .F. ) ;
#10727 = ORIENTED_EDGE ( 'NONE', *, *, #5371, .F. ) ;
#10728 = ORIENTED_EDGE ( 'NONE', *, *, #1484, .F. ) ;
#10729 = CARTESIAN_POINT ( 'NONE',  ( 0.000000000000000000, 0.007874015748031480341, 0.5826771653543306728 ) ) ;
#10730 = CARTESIAN_POINT ( 'NONE',  ( -1.932153213347265197, -2.929935046723639580, -0.08117000303833375729 ) ) ;
#10731 = CARTESIAN_POINT ( 'NONE',  ( 0.05175539059627461136, 0.000000000000000000, -0.07475334604056278753 ) ) ;
#10732 = DIRECTION ( 'NONE',  ( 0.000000000000000000, 0.000000000000000000, -1.000000000000000000 ) ) ;
#10733 = DIRECTION ( 'NONE',  ( -0.000000000000000000, -1.000000000000000000, -0.000000000000000000 ) ) ;
#10734 = DIRECTION ( 'NONE',  ( 0.000000000000000000, 0.000000000000000000, -1.000000000000000000 ) ) ;
#10735 = CARTESIAN_POINT ( 'NONE',  ( -2.018747272517074531, -2.567808539723777983, 0.1539156967279681487 ) ) ;
#10736 = ORIENTED_EDGE ( 'NONE', *, *, #6875, .F. ) ;
#10737 = CARTESIAN_POINT ( 'NONE',  ( -1.953932514027914014, -2.911092722762949059, -0.08698641157505102028 ) ) ;
#10738 = CARTESIAN_POINT ( 'NONE',  ( -0.06012940348033157800, 1.340161119985692872, -0.5902917039295724200 ) ) ;
#10739 = DIRECTION ( 'NONE',  ( 0.000000000000000000, 0.000000000000000000, -1.000000000000000000 ) ) ;
#10740 = CARTESIAN_POINT ( 'NONE',  ( 0.2681506793018588741, -0.1023622047244094474, 0.03207310886168002889 ) ) ;
#10741 = ORIENTED_EDGE ( 'NONE', *, *, #13739, .F. ) ;
#10742 = EDGE_CURVE ( 'NONE', #6761, #7284, #9484, .T. ) ;
#10743 = EDGE_CURVE ( 'NONE', #11638, #8739, #11981, .T. ) ;
#10744 = ORIENTED_EDGE ( 'NONE', *, *, #7114, .F. ) ;
#10745 = ORIENTED_EDGE ( 'NONE', *, *, #5129, .T. ) ;
#10746 = EDGE_CURVE ( 'NONE', #897, #13132, #7955, .T. ) ;
#10747 = CARTESIAN_POINT ( 'NONE',  ( -0.06692913385815735250, -0.4881889763779528324, -0.5870514566507987197 ) ) ;
#10748 = CARTESIAN_POINT ( 'NONE',  ( -1.419615703680148000, -0.01226548409420234569, 0.07874015748031495954 ) ) ;
#10749 = DIRECTION ( 'NONE',  ( 0.000000000000000000, 0.000000000000000000, 1.000000000000000000 ) ) ;
#10750 = CARTESIAN_POINT ( 'NONE',  ( -0.3441669734936866343, 2.010494531933507467, 0.05905511811023622659 ) ) ;
#10751 = CARTESIAN_POINT ( 'NONE',  ( 2.025006518275150778E-17, 0.007874015748031480341, -0.1653543307086614012 ) ) ;
#10752 = ORIENTED_EDGE ( 'NONE', *, *, #10385, .T. ) ;
#10753 = CARTESIAN_POINT ( 'NONE',  ( -1.580080891953811628, 0.1020406297922293176, -0.07874015748031495954 ) ) ;
#10754 = DIRECTION ( 'NONE',  ( 0.8660254037844385966, 0.000000000000000000, 0.5000000000000000000 ) ) ;
#10755 = DIRECTION ( 'NONE',  ( 3.973232667114494807E-16, -0.000000000000000000, -1.000000000000000000 ) ) ;
#10756 = CARTESIAN_POINT ( 'NONE',  ( -0.06145017734370220031, -0.1666692956086705812, 0.05763041683086380512 ) ) ;
#10757 = EDGE_CURVE ( 'NONE', #9271, #13131, #8721, .T. ) ;
#10758 = DIRECTION ( 'NONE',  ( 1.000000000000000000, 0.000000000000000000, 1.445602896647339903E-16 ) ) ;
#10759 = EDGE_CURVE ( 'NONE', #897, #3157, #2712, .T. ) ;
#10760 = ORIENTED_EDGE ( 'NONE', *, *, #6196, .T. ) ;
#10761 = EDGE_LOOP ( 'NONE', ( #4084, #4698 ) ) ;
#10762 = VERTEX_POINT ( 'NONE', #9250 ) ;
#10763 = ORIENTED_EDGE ( 'NONE', *, *, #3571, .F. ) ;
#10764 = EDGE_CURVE ( 'NONE', #14809, #1289, #3211, .T. ) ;
#10765 = EDGE_CURVE ( 'NONE', #1514, #12673, #225, .T. ) ;
#10766 = CARTESIAN_POINT ( 'NONE',  ( -0.1023622047242991884, -0.2952755905511811885, -0.3757906139821208802 ) ) ;
#10767 = CARTESIAN_POINT ( 'NONE',  ( -1.897873245346056947, -2.949503897763099403, -0.005687192277569496669 ) ) ;
#10768 = DIRECTION ( 'NONE',  ( 0.7118260687460293834, 0.5695655044020487834, -0.4109729724067173739 ) ) ;
#10769 = DIRECTION ( 'NONE',  ( 0.000000000000000000, 1.000000000000000000, 0.000000000000000000 ) ) ;
#10770 = DIRECTION ( 'NONE',  ( 1.000000000000000000, 0.000000000000000000, 0.000000000000000000 ) ) ;
#10771 = FACE_OUTER_BOUND ( 'NONE', #9973, .T. ) ;
#10772 = PLANE ( 'NONE',  #14889 ) ;
#10773 = CARTESIAN_POINT ( 'NONE',  ( 0.4625984251968510708, -0.4881889763779528324, 0.3807329531073309070 ) ) ;
#10774 = FACE_OUTER_BOUND ( 'NONE', #11718, .T. ) ;
#10775 = VERTEX_POINT ( 'NONE', #10196 ) ;
#10776 = ORIENTED_EDGE ( 'NONE', *, *, #11015, .T. ) ;
#10777 = ORIENTED_EDGE ( 'NONE', *, *, #13532, .F. ) ;
#10778 = ORIENTED_EDGE ( 'NONE', *, *, #2261, .T. ) ;
#10779 = EDGE_CURVE ( 'NONE', #13855, #2421, #2214, .T. ) ;
#10780 = ADVANCED_FACE ( 'NONE', ( #5478 ), #15207, .F. ) ;
#10781 = CARTESIAN_POINT ( 'NONE',  ( -2.100501784635051550, -1.630597114118274238, -0.1033464566929129386 ) ) ;
#10782 = CARTESIAN_POINT ( 'NONE',  ( -1.945459748359986252, -2.745801194614591711, 0.1561691687464105693 ) ) ;
#10783 = LINE ( 'NONE', #8580, #6668 ) ;
#10784 = EDGE_CURVE ( 'NONE', #11091, #1695, #7867, .T. ) ;
#10785 = DIRECTION ( 'NONE',  ( -0.6461174802841006537, 0.7632379718484431086, -1.126465149071359074E-12 ) ) ;
#10786 = FACE_OUTER_BOUND ( 'NONE', #473, .T. ) ;
#10787 = CARTESIAN_POINT ( 'NONE',  ( -1.398125690441303526, -0.003404927804347070153, 0.05905511811023622659 ) ) ;
#10788 = ORIENTED_EDGE ( 'NONE', *, *, #8214, .T. ) ;
#10789 = FACE_OUTER_BOUND ( 'NONE', #1485, .T. ) ;
#10790 = DIRECTION ( 'NONE',  ( -3.973232667114494807E-16, 0.000000000000000000, 1.000000000000000000 ) ) ;
#10791 = DIRECTION ( 'NONE',  ( -1.000000000000000000, 0.000000000000000000, 0.000000000000000000 ) ) ;
#10792 = ORIENTED_EDGE ( 'NONE', *, *, #12282, .T. ) ;
#10793 = VERTEX_POINT ( 'NONE', #13791 ) ;
#10794 = ORIENTED_EDGE ( 'NONE', *, *, #1868, .F. ) ;
#10795 = CARTESIAN_POINT ( 'NONE',  ( -2.168820329264121050, -1.823085014281403016, 0.1033464566929129386 ) ) ;
#10796 = CARTESIAN_POINT ( 'NONE',  ( 0.000000000000000000, -0.4921259842519685179, 0.000000000000000000 ) ) ;
#10797 = ADVANCED_FACE ( 'NONE', ( #4469 ), #15118, .F. ) ;
#10798 = CARTESIAN_POINT ( 'NONE',  ( -1.253866366384063902, 0.1355266887446167634, -0.03937007874015747977 ) ) ;
#10799 = CARTESIAN_POINT ( 'NONE',  ( 0.000000000000000000, 1.661417322834646049, 0.000000000000000000 ) ) ;
#10800 = DIRECTION ( 'NONE',  ( 0.000000000000000000, 1.000000000000000000, 0.000000000000000000 ) ) ;
#10801 = CARTESIAN_POINT ( 'NONE',  ( -1.930616173493556520, -2.788983622150487118, 0.1558567757490539607 ) ) ;
#10802 = ORIENTED_EDGE ( 'NONE', *, *, #12484, .F. ) ;
#10803 = CARTESIAN_POINT ( 'NONE',  ( 0.000000000000000000, 1.409448818897637956, -0.5590551181102362266 ) ) ;
#10804 = CARTESIAN_POINT ( 'NONE',  ( -1.181102362204724310, 0.1240157480314959815, -0.02952755905511811330 ) ) ;
#10805 = ORIENTED_EDGE ( 'NONE', *, *, #14623, .F. ) ;
#10806 = ORIENTED_EDGE ( 'NONE', *, *, #8453, .T. ) ;
#10807 = VERTEX_POINT ( 'NONE', #2269 ) ;
#10808 = CARTESIAN_POINT ( 'NONE',  ( 0.1017691531708310448, -0.2952755905511811330, 0.7406662147377752747 ) ) ;
#10809 = FACE_OUTER_BOUND ( 'NONE', #6058, .T. ) ;
#10810 = DIRECTION ( 'NONE',  ( -0.000000000000000000, 1.000000000000000000, -0.000000000000000000 ) ) ;
#10811 = CARTESIAN_POINT ( 'NONE',  ( -0.06299212598414161146, -0.4921259842519685179, -0.5870514566507987197 ) ) ;
#10812 = DIRECTION ( 'NONE',  ( 0.000000000000000000, 0.000000000000000000, -1.000000000000000000 ) ) ;
#10813 = EDGE_CURVE ( 'NONE', #12795, #5281, #5945, .T. ) ;
#10814 = DIRECTION ( 'NONE',  ( -0.000000000000000000, -1.000000000000000000, -0.000000000000000000 ) ) ;
#10815 = ORIENTED_EDGE ( 'NONE', *, *, #8490, .F. ) ;
#10816 = CARTESIAN_POINT ( 'NONE',  ( -1.606548329185371937, 0.09883514492710566979, -0.06506891156476989069 ) ) ;
#10817 = LINE ( 'NONE', #266, #10645 ) ;
#10818 = TOROIDAL_SURFACE ( 'NONE', #9847, 0.5984251968503937480, 0.007874015748031495954 ) ;
#10819 = DIRECTION ( 'NONE',  ( 2.664535259100375697E-15, 0.000000000000000000, -1.000000000000000000 ) ) ;
#10820 = EDGE_CURVE ( 'NONE', #11532, #13926, #6198, .T. ) ;
#10821 = DIRECTION ( 'NONE',  ( 0.5000000000000004441, -0.000000000000000000, -0.8660254037844384856 ) ) ;
#10822 = EDGE_LOOP ( 'NONE', ( #10187, #162, #15014 ) ) ;
#10823 = VERTEX_POINT ( 'NONE', #6975 ) ;
#10824 = ORIENTED_EDGE ( 'NONE', *, *, #1481, .T. ) ;
#10825 = ORIENTED_EDGE ( 'NONE', *, *, #9588, .F. ) ;
#10826 = FACE_OUTER_BOUND ( 'NONE', #4660, .T. ) ;
#10827 = VECTOR ( 'NONE', #6023, 39.37007874015748143 ) ;
#10828 = CIRCLE ( 'NONE', #5313, 0.003937007874015750579 ) ;
#10829 = AXIS2_PLACEMENT_3D ( 'NONE', #1002, #9221, #2306 ) ;
#10830 = FACE_OUTER_BOUND ( 'NONE', #11303, .T. ) ;
#10831 = DIRECTION ( 'NONE',  ( 1.000000000000000000, 0.000000000000000000, 0.000000000000000000 ) ) ;
#10832 = EDGE_CURVE ( 'NONE', #11006, #12201, #7044, .T. ) ;
#10833 = VECTOR ( 'NONE', #4933, 39.37007874015748143 ) ;
#10834 = DIRECTION ( 'NONE',  ( -0.7118260687460293834, 0.5695655044020491165, -0.4109729724067171519 ) ) ;
#10835 = DIRECTION ( 'NONE',  ( -0.5000000000000001110, 0.000000000000000000, 0.8660254037844385966 ) ) ;
#10836 = EDGE_CURVE ( 'NONE', #2901, #8551, #955, .T. ) ;
#10837 = CARTESIAN_POINT ( 'NONE',  ( -0.06299212598414173636, -0.1023622047244094474, -0.2377126739438355507 ) ) ;
#10838 = CARTESIAN_POINT ( 'NONE',  ( -0.4307978335858689278, -0.09448818897637796532, 0.4318761856142863120 ) ) ;
#10839 = DIRECTION ( 'NONE',  ( -1.000000000000000000, 0.000000000000000000, 0.000000000000000000 ) ) ;
#10840 = EDGE_CURVE ( 'NONE', #13129, #1428, #13472, .T. ) ;
#10841 = CARTESIAN_POINT ( 'NONE',  ( -1.964126537190518107, -2.749515453455440905, 0.1756903148397124803 ) ) ;
#10842 = DIRECTION ( 'NONE',  ( 0.000000000000000000, 0.000000000000000000, 1.000000000000000000 ) ) ;
#10843 = AXIS2_PLACEMENT_3D ( 'NONE', #13138, #9542, #5994 ) ;
#10844 = AXIS2_PLACEMENT_3D ( 'NONE', #4428, #9215, #7720 ) ;
#10845 = ORIENTED_EDGE ( 'NONE', *, *, #11709, .T. ) ;
#10846 = AXIS2_PLACEMENT_3D ( 'NONE', #2038, #6737, #11526 ) ;
#10847 = VECTOR ( 'NONE', #5567, 39.37007874015748143 ) ;
#10848 = ORIENTED_EDGE ( 'NONE', *, *, #3697, .T. ) ;
#10849 = ORIENTED_EDGE ( 'NONE', *, *, #2420, .F. ) ;
#10850 = ADVANCED_FACE ( 'NONE', ( #8153 ), #14263, .T. ) ;
#10851 = CARTESIAN_POINT ( 'NONE',  ( 0.000000000000000000, -0.4881889763779528324, -0.1535433070866141780 ) ) ;
#10852 = DIRECTION ( 'NONE',  ( 0.8660254037844362651, 0.000000000000000000, -0.5000000000000038858 ) ) ;
#10853 = VECTOR ( 'NONE', #14560, 39.37007874015748143 ) ;
#10854 = CIRCLE ( 'NONE', #10353, 0.03937007874015751446 ) ;
#10855 = EDGE_CURVE ( 'NONE', #426, #2689, #13166, .T. ) ;
#10856 = CYLINDRICAL_SURFACE ( 'NONE', #13714, 0.003937007874015749712 ) ;
#10857 = DIRECTION ( 'NONE',  ( 0.8660254037844365982, -0.000000000000000000, 0.5000000000000035527 ) ) ;
#10858 = TOROIDAL_SURFACE ( 'NONE', #10121, 0.5826771653543306728, 0.007874015748031495954 ) ;
#10859 = DIRECTION ( 'NONE',  ( -0.7666137478421605200, 0.6421085279136201640, 0.000000000000000000 ) ) ;
#10860 = CIRCLE ( 'NONE', #3108, 0.03937007874015747977 ) ;
#10861 = B_SPLINE_CURVE_WITH_KNOTS ( 'NONE', 3,
 ( #5834, #11750, #1013, #3441, #2253, #4690 ),
 .UNSPECIFIED., .F., .F.,
 ( 4, 2, 4 ),
 ( -2.828444569871933696E-06, 0.0001777364543001176602, 0.0003583013531701072511 ),
 .UNSPECIFIED. ) ;
#10862 = CARTESIAN_POINT ( 'NONE',  ( 0.1023622047244638761, -0.2952755905511811330, -0.4190977005962941426 ) ) ;
#10863 = AXIS2_PLACEMENT_3D ( 'NONE', #14531, #10920, #4965 ) ;
#10864 = DIRECTION ( 'NONE',  ( -0.8660254037844428154, 0.000000000000000000, -0.4999999999999926725 ) ) ;
#10865 = EDGE_CURVE ( 'NONE', #6453, #562, #6457, .T. ) ;
#10866 = CYLINDRICAL_SURFACE ( 'NONE', #9084, 0.03937007874015751446 ) ;
#10867 = CARTESIAN_POINT ( 'NONE',  ( 0.4859532342797860394, 1.043307086614173373, 0.3487562073009374264 ) ) ;
#10868 = ORIENTED_EDGE ( 'NONE', *, *, #9538, .T. ) ;
#10869 = ORIENTED_EDGE ( 'NONE', *, *, #11860, .T. ) ;
#10870 = CIRCLE ( 'NONE', #9383, 0.007874015748031516770 ) ;
#10871 = AXIS2_PLACEMENT_3D ( 'NONE', #6779, #765, #11569 ) ;
#10872 = AXIS2_PLACEMENT_3D ( 'NONE', #2170, #13120, #3259 ) ;
#10873 = CIRCLE ( 'NONE', #1377, 0.003937007874015721089 ) ;
#10874 = EDGE_CURVE ( 'NONE', #8556, #11565, #7185, .T. ) ;
#10875 = EDGE_LOOP ( 'NONE', ( #6056, #4494 ) ) ;
#10876 = AXIS2_PLACEMENT_3D ( 'NONE', #9018, #4006, #1888 ) ;
#10877 = DIRECTION ( 'NONE',  ( 0.000000000000000000, -0.000000000000000000, -1.000000000000000000 ) ) ;
#10878 = CARTESIAN_POINT ( 'NONE',  ( -1.602629991056265801, 0.1043896402809140617, 0.05327537141218099959 ) ) ;
#10879 = CARTESIAN_POINT ( 'NONE',  ( 0.06692913385832208184, -0.2952755905511811330, -0.3797276218561366212 ) ) ;
#10880 = CARTESIAN_POINT ( 'NONE',  ( -0.5445274672588088505, 1.043263280880422528, 0.2461921031270815630 ) ) ;
#10881 = DIRECTION ( 'NONE',  ( -0.5000000000000000000, -0.000000000000000000, -0.8660254037844388186 ) ) ;
#10882 = AXIS2_PLACEMENT_3D ( 'NONE', #14967, #3123, #10488 ) ;
#10883 = DIRECTION ( 'NONE',  ( 1.000000000000000000, -0.000000000000000000, 0.000000000000000000 ) ) ;
#10884 = AXIS2_PLACEMENT_3D ( 'NONE', #14837, #1687, #9043 ) ;
#10885 = CARTESIAN_POINT ( 'NONE',  ( -1.904888967627721863, -2.858900249894324119, 0.1271124878405535397 ) ) ;
#10886 = VERTEX_POINT ( 'NONE', #11765 ) ;
#10887 = CARTESIAN_POINT ( 'NONE',  ( -1.951376757933277917, -2.917415184539839945, 0.07729597236840124452 ) ) ;
#10888 = EDGE_CURVE ( 'NONE', #1202, #12059, #1229, .T. ) ;
#10889 = VECTOR ( 'NONE', #13223, 39.37007874015748143 ) ;
#10890 = DIRECTION ( 'NONE',  ( 0.000000000000000000, 1.000000000000000000, 0.000000000000000000 ) ) ;
#10891 = ORIENTED_EDGE ( 'NONE', *, *, #7160, .F. ) ;
#10892 = VERTEX_POINT ( 'NONE', #11924 ) ;
#10893 = EDGE_CURVE ( 'NONE', #12689, #15156, #445, .T. ) ;
#10894 = ADVANCED_FACE ( 'NONE', ( #5777 ), #10570, .T. ) ;
#10896 = VERTEX_POINT ( 'NONE', #15 ) ;
#10895 = AXIS2_PLACEMENT_3D ( 'NONE', #13519, #13290, #12129 ) ;
#10897 = CIRCLE ( 'NONE', #12151, 0.003937007874015749712 ) ;
#10898 = B_SPLINE_CURVE_WITH_KNOTS ( 'NONE', 3,
 ( #8906, #1768, #13823, #3256, #754, #7870 ),
 .UNSPECIFIED., .F., .F.,
 ( 4, 2, 4 ),
 ( 1.390486644391990834E-17, 0.01145241905537470843, 0.02290483811074940299 ),
 .UNSPECIFIED. ) ;
#10899 = TOROIDAL_SURFACE ( 'NONE', #9916, 0.007874015748031495954, 0.003937007874015747977 ) ;
#10900 = DIRECTION ( 'NONE',  ( 1.000000000000000000, 0.000000000000000000, -0.000000000000000000 ) ) ;
#10901 = AXIS2_PLACEMENT_3D ( 'NONE', #12811, #3428, #10702 ) ;
#10902 = CARTESIAN_POINT ( 'NONE',  ( -0.05905511811023622659, 1.043012312267831421, -0.5922897223582480608 ) ) ;
#10903 = CARTESIAN_POINT ( 'NONE',  ( -0.3964138223131424277, -0.2952755905511811330, 0.1515865201236452631 ) ) ;
#10904 = CARTESIAN_POINT ( 'NONE',  ( 0.1618514667033794374, -0.1023622047244094474, 0.2161887458866224576 ) ) ;
#10905 = CARTESIAN_POINT ( 'NONE',  ( -0.08151194962748890827, 0.1637246173173402264, -0.03937007874015747977 ) ) ;
#10906 = EDGE_LOOP ( 'NONE', ( #14824, #379, #5713, #11213 ) ) ;
#10907 = DIRECTION ( 'NONE',  ( 0.000000000000000000, 0.000000000000000000, 1.000000000000000000 ) ) ;
#10908 = DIRECTION ( 'NONE',  ( -0.4999999999999967804, -0.000000000000000000, -0.8660254037844405950 ) ) ;
#10909 = AXIS2_PLACEMENT_3D ( 'NONE', #2829, #7614, #12407 ) ;
#10910 = AXIS2_PLACEMENT_3D ( 'NONE', #11177, #9851, #6291 ) ;
#10911 = CARTESIAN_POINT ( 'NONE',  ( -0.07635964791965738074, -0.1878198040935885327, 0.03937007874015747977 ) ) ;
#10912 = VECTOR ( 'NONE', #15149, 39.37007874015748143 ) ;
#10913 = ORIENTED_EDGE ( 'NONE', *, *, #12678, .T. ) ;
#10914 = ORIENTED_EDGE ( 'NONE', *, *, #8780, .F. ) ;
#10915 = EDGE_LOOP ( 'NONE', ( #5166, #10439, #12445, #1424 ) ) ;
#10916 = ORIENTED_EDGE ( 'NONE', *, *, #1778, .T. ) ;
#10917 = CARTESIAN_POINT ( 'NONE',  ( -1.588328939002294549, 0.1239872266390840139, -0.03937007874015752834 ) ) ;
#10918 = AXIS2_PLACEMENT_3D ( 'NONE', #5034, #5118, #1598 ) ;
#10919 = DIRECTION ( 'NONE',  ( -0.000000000000000000, 0.000000000000000000, 1.000000000000000000 ) ) ;
#10920 = DIRECTION ( 'NONE',  ( -0.4333736175764353327, 0.8657846595920662969, 0.2502083747674392900 ) ) ;
#10921 = CARTESIAN_POINT ( 'NONE',  ( -1.415143637612825467, -0.009756740514708567291, 0.06578375869326227865 ) ) ;
#10922 = AXIS2_PLACEMENT_3D ( 'NONE', #4953, #12081, #10907 ) ;
#10923 = CYLINDRICAL_SURFACE ( 'NONE', #11893, 0.003937007874015749712 ) ;
#10924 = FACE_OUTER_BOUND ( 'NONE', #3465, .T. ) ;
#10925 = LINE ( 'NONE', #15409, #11586 ) ;
#10926 = DIRECTION ( 'NONE',  ( 0.000000000000000000, 1.000000000000000000, 0.000000000000000000 ) ) ;
#10927 = CARTESIAN_POINT ( 'NONE',  ( -1.387704745771440207, -0.02010536753476152225, 0.03937007874015747977 ) ) ;
#10928 = CYLINDRICAL_SURFACE ( 'NONE', #1172, 0.003937007874015758385 ) ;
#10929 = CIRCLE ( 'NONE', #1434, 0.5984251968503937480 ) ;
#10930 = VERTEX_POINT ( 'NONE', #15355 ) ;
#10931 = EDGE_CURVE ( 'NONE', #677, #3049, #1725, .T. ) ;
#10932 = EDGE_LOOP ( 'NONE', ( #10825, #7358, #1142, #12807 ) ) ;
#10933 = AXIS2_PLACEMENT_3D ( 'NONE', #13226, #3, #8515 ) ;
#10934 = EDGE_CURVE ( 'NONE', #924, #12712, #2430, .T. ) ;
#10935 = ORIENTED_EDGE ( 'NONE', *, *, #5571, .F. ) ;
#10936 = AXIS2_PLACEMENT_3D ( 'NONE', #11707, #4558, #8178 ) ;
#10937 = EDGE_CURVE ( 'NONE', #6761, #15201, #4620, .T. ) ;
#10938 = DIRECTION ( 'NONE',  ( 0.5000000000000069944, 0.000000000000000000, -0.8660254037844347108 ) ) ;
#10939 = DIRECTION ( 'NONE',  ( -1.000000000000000000, 0.000000000000000000, 0.000000000000000000 ) ) ;
#10940 = AXIS2_PLACEMENT_3D ( 'NONE', #4053, #13932, #477 ) ;
#10941 = DIRECTION ( 'NONE',  ( -1.000000000000000000, 0.000000000000000000, 0.000000000000000000 ) ) ;
#10942 = CARTESIAN_POINT ( 'NONE',  ( -1.100415514366371195, -0.04998955061625851709, -0.03937007874015747977 ) ) ;
#10943 = DIRECTION ( 'NONE',  ( 1.000000000000000000, 0.000000000000000000, 0.000000000000000000 ) ) ;
#10944 = CIRCLE ( 'NONE', #1694, 0.04330708661417329020 ) ;
#10945 = DIRECTION ( 'NONE',  ( 1.000000000000000000, 0.000000000000000000, 0.000000000000000000 ) ) ;
#10946 = FACE_OUTER_BOUND ( 'NONE', #1529, .T. ) ;
#10947 = CARTESIAN_POINT ( 'NONE',  ( -0.06351958502436047538, -0.4921259842519685179, -0.2357441700068276802 ) ) ;
#10948 = VERTEX_POINT ( 'NONE', #5707 ) ;
#10949 = ADVANCED_FACE ( 'NONE', ( #9647 ), #14187, .F. ) ;
#10950 = ORIENTED_EDGE ( 'NONE', *, *, #10958, .F. ) ;
#10951 = AXIS2_PLACEMENT_3D ( 'NONE', #9934, #14626, #292 ) ;
#10952 = ORIENTED_EDGE ( 'NONE', *, *, #1943, .T. ) ;
#10953 = EDGE_CURVE ( 'NONE', #9541, #4974, #10499, .T. ) ;
#10954 = ORIENTED_EDGE ( 'NONE', *, *, #6988, .F. ) ;
#10955 = ORIENTED_EDGE ( 'NONE', *, *, #14997, .T. ) ;
#10956 = CIRCLE ( 'NONE', #1222, 0.5984251968503937480 ) ;
#10957 = CARTESIAN_POINT ( 'NONE',  ( -0.3314531923919099565, -0.2952755905511811330, 0.2641016316388978824 ) ) ;
#10958 = EDGE_CURVE ( 'NONE', #10886, #15338, #5859, .T. ) ;
#10959 = ADVANCED_FACE ( 'NONE', ( #12232, #3993, #5063 ), #5226, .T. ) ;
#10960 = DIRECTION ( 'NONE',  ( 0.000000000000000000, -1.000000000000000000, -0.000000000000000000 ) ) ;
#10961 = LINE ( 'NONE', #9867, #1635 ) ;
#10962 = CARTESIAN_POINT ( 'NONE',  ( 0.000000000000000000, 0.003937007874015749712, 0.000000000000000000 ) ) ;
#10964 = AXIS2_PLACEMENT_3D ( 'NONE', #4296, #785, #9089 ) ;
#10963 = CARTESIAN_POINT ( 'NONE',  ( -1.190198933766852152, 0.3259758027579607309, 0.05905511811023622659 ) ) ;
#10965 = CARTESIAN_POINT ( 'NONE',  ( -1.913690542245347626, -2.905358729579917476, -0.1176961216033449859 ) ) ;
#10966 = EDGE_LOOP ( 'NONE', ( #12873, #7158, #8073, #12753 ) ) ;
#10967 = CARTESIAN_POINT ( 'NONE',  ( -1.947386292800456387, -2.927198029129052692, 0.05659550234681299391 ) ) ;
#10968 = CARTESIAN_POINT ( 'NONE',  ( -0.3746568166374384945, -0.2952755905511811330, 0.1026565861461826018 ) ) ;
#10969 =( GEOMETRIC_REPRESENTATION_CONTEXT ( 3 ) GLOBAL_UNCERTAINTY_ASSIGNED_CONTEXT ( ( #11276 ) ) GLOBAL_UNIT_ASSIGNED_CONTEXT ( ( #11246, #521, #11167 ) ) REPRESENTATION_CONTEXT ( 'NONE', 'WORKASPACE' ) );
#10970 = FACE_BOUND ( 'NONE', #9856, .T. ) ;
#10971 = EDGE_LOOP ( 'NONE', ( #13017, #6792, #9127, #966 ) ) ;
#10972 = EDGE_LOOP ( 'NONE', ( #4481, #8435, #5453, #9679 ) ) ;
#10973 = EDGE_LOOP ( 'NONE', ( #1715, #4879, #3804, #13697, #1016, #2788, #13837, #827 ) ) ;
#10974 = CARTESIAN_POINT ( 'NONE',  ( 0.000000000000000000, 1.377952755905512028, 0.000000000000000000 ) ) ;
#10975 = EDGE_CURVE ( 'NONE', #9581, #2107, #6414, .T. ) ;
#10976 = DIRECTION ( 'NONE',  ( 0.000000000000000000, 0.000000000000000000, 1.000000000000000000 ) ) ;
#10977 = FACE_OUTER_BOUND ( 'NONE', #12305, .T. ) ;
#10978 = CARTESIAN_POINT ( 'NONE',  ( 0.06604848736013260724, 1.346456692913385877, -0.5868460571724354313 ) ) ;
#10979 = CONTEXT_DEPENDENT_SHAPE_REPRESENTATION ( #15017, #12923 ) ;
#10980 = CYLINDRICAL_SURFACE ( 'NONE', #695, 0.007874015748031516770 ) ;
#10981 = DIRECTION ( 'NONE',  ( 0.000000000000000000, 0.000000000000000000, 1.000000000000000000 ) ) ;
#10982 = CARTESIAN_POINT ( 'NONE',  ( -0.05270315828015969400, 0.1680450278838720168, -0.03205052537796104772 ) ) ;
#10983 = VERTEX_POINT ( 'NONE', #13393 ) ;
#10984 = CARTESIAN_POINT ( 'NONE',  ( -1.398495881576244493, -0.02731002314121875815, -0.08366141732283458032 ) ) ;
#10985 = EDGE_CURVE ( 'NONE', #4739, #12623, #1643, .T. ) ;
#10986 = FACE_OUTER_BOUND ( 'NONE', #9425, .T. ) ;
#10987 = CARTESIAN_POINT ( 'NONE',  ( -1.181102362204724310, 0.000000000000000000, -0.02559055118110236185 ) ) ;
#10988 = CARTESIAN_POINT ( 'NONE',  ( 0.4516353949179792160, -0.2952755905511811330, 0.1425541239265584736 ) ) ;
#10989 = FACE_OUTER_BOUND ( 'NONE', #14265, .T. ) ;
#10990 = ORIENTED_EDGE ( 'NONE', *, *, #8495, .F. ) ;
#10991 = ORIENTED_EDGE ( 'NONE', *, *, #9517, .T. ) ;
#10992 = ORIENTED_EDGE ( 'NONE', *, *, #8063, .F. ) ;
#10993 = VERTEX_POINT ( 'NONE', #8698 ) ;
#10994 = CARTESIAN_POINT ( 'NONE',  ( 0.000000000000000000, 0.5826771653543306728, 0.000000000000000000 ) ) ;
#10995 = CARTESIAN_POINT ( 'NONE',  ( 0.6864776960422569463, 1.043307086614173151, 0.4645290592786023298 ) ) ;
#10996 = DIRECTION ( 'NONE',  ( 1.000000000000000000, 0.000000000000000000, 3.075191616504340279E-15 ) ) ;
#10997 = DIRECTION ( 'NONE',  ( 0.000000000000000000, 1.000000000000000000, 0.000000000000000000 ) ) ;
#10998 = DIRECTION ( 'NONE',  ( 0.4932581959314703557, 0.8219459448134283086, 0.2847827522010267787 ) ) ;
#10999 = DIRECTION ( 'NONE',  ( -0.8660254037844398178, 0.000000000000000000, 0.4999999999999979461 ) ) ;
#11000 = CYLINDRICAL_SURFACE ( 'NONE', #1356, 0.003937007874015721089 ) ;
#11001 = CARTESIAN_POINT ( 'NONE',  ( -1.181102362204724310, 0.1279527559055117225, -0.02559055118110236185 ) ) ;
#11002 = EDGE_CURVE ( 'NONE', #1695, #5321, #4465, .T. ) ;
#11003 = DIRECTION ( 'NONE',  ( 0.8660254037844390407, 0.000000000000000000, -0.4999999999999990008 ) ) ;
#11004 = CARTESIAN_POINT ( 'NONE',  ( -0.05905511811023622659, 1.190944881889763884, -0.8267716535433072833 ) ) ;
#11005 = ORIENTED_EDGE ( 'NONE', *, *, #2020, .F. ) ;
#11006 = VERTEX_POINT ( 'NONE', #5149 ) ;
#11007 = EDGE_LOOP ( 'NONE', ( #3412, #13464, #12903, #11936 ) ) ;
#11008 = CARTESIAN_POINT ( 'NONE',  ( -2.065879816533417124, -2.386386741922390531, -0.1342549684437943924 ) ) ;
#11009 = CARTESIAN_POINT ( 'NONE',  ( -1.941126393898428226, -2.942417223422608252, -0.04999253742952749352 ) ) ;
#11010 = CARTESIAN_POINT ( 'NONE',  ( -2.163017314575554462, -1.630597114118274238, 0.08366141732283423338 ) ) ;
#11011 = DIRECTION ( 'NONE',  ( -0.5000000000000000000, 0.000000000000000000, 0.8660254037844385966 ) ) ;
#11012 = CARTESIAN_POINT ( 'NONE',  ( 0.000000000000000000, 0.4094488188976377896, 0.03543307086614173179 ) ) ;
#11013 = CARTESIAN_POINT ( 'NONE',  ( -1.181102362204724310, 0.1240157480314959815, -0.02559055118110236185 ) ) ;
#11014 = FACE_BOUND ( 'NONE', #8774, .T. ) ;
#11015 = EDGE_CURVE ( 'NONE', #4061, #7217, #2660, .T. ) ;
#11016 = DIRECTION ( 'NONE',  ( 1.000000000000000000, 0.000000000000000000, 0.000000000000000000 ) ) ;
#11017 = DIRECTION ( 'NONE',  ( -0.8660254037844389297, -0.000000000000000000, 0.4999999999999994449 ) ) ;
#11018 = FACE_OUTER_BOUND ( 'NONE', #1830, .T. ) ;
#11019 = VERTEX_POINT ( 'NONE', #9726 ) ;
#11020 = ADVANCED_FACE ( 'NONE', ( #13239 ), #13471, .T. ) ;
#11021 = ORIENTED_EDGE ( 'NONE', *, *, #14113, .F. ) ;
#11022 = ORIENTED_EDGE ( 'NONE', *, *, #948, .T. ) ;
#11023 = EDGE_LOOP ( 'NONE', ( #14589, #12352, #548, #13674 ) ) ;
#11024 = ORIENTED_EDGE ( 'NONE', *, *, #3011, .F. ) ;
#11025 = FACE_OUTER_BOUND ( 'NONE', #11007, .T. ) ;
#11026 = DIRECTION ( 'NONE',  ( -0.000000000000000000, -2.212657494868377674E-16, -1.000000000000000000 ) ) ;
#11027 = EDGE_CURVE ( 'NONE', #5052, #14569, #4433, .T. ) ;
#11028 = DIRECTION ( 'NONE',  ( 1.000000000000000000, 0.000000000000000000, 0.000000000000000000 ) ) ;
#11029 = DIRECTION ( 'NONE',  ( 4.257580834543280144E-32, 1.000000000000000000, -1.224646799147353207E-16 ) ) ;
#11030 = CARTESIAN_POINT ( 'NONE',  ( -1.898519999023877469, -2.947734826116759965, -0.02574579424190774277 ) ) ;
#11031 = EDGE_CURVE ( 'NONE', #7482, #517, #14737, .T. ) ;
#11032 = VERTEX_POINT ( 'NONE', #1492 ) ;
#11033 = CARTESIAN_POINT ( 'NONE',  ( 0.05114323250695503031, 0.05905511811023622659, 0.08858267716535433989 ) ) ;
#11034 = DIRECTION ( 'NONE',  ( 1.000000000000000000, 0.000000000000000000, 8.673617379884028570E-16 ) ) ;
#11035 = DIRECTION ( 'NONE',  ( -0.8660254037844388186, 0.000000000000000000, 0.4999999999999995559 ) ) ;
#11036 = ORIENTED_EDGE ( 'NONE', *, *, #580, .F. ) ;
#11037 = EDGE_CURVE ( 'NONE', #8021, #5345, #1967, .T. ) ;
#11038 = EDGE_LOOP ( 'NONE', ( #14140, #13061, #10455, #10891 ) ) ;
#11039 = ORIENTED_EDGE ( 'NONE', *, *, #1175, .F. ) ;
#11040 = LINE ( 'NONE', #2748, #14366 ) ;
#11041 = LINE ( 'NONE', #2583, #633 ) ;
#11042 = DIRECTION ( 'NONE',  ( 0.000000000000000000, 0.000000000000000000, -1.000000000000000000 ) ) ;
#11043 = CARTESIAN_POINT ( 'NONE',  ( -0.007978440472143270498, -0.1611588996411620900, -0.01594766689393424530 ) ) ;
#11044 = ADVANCED_FACE ( 'NONE', ( #14498 ), #9869, .T. ) ;
#11045 = ORIENTED_EDGE ( 'NONE', *, *, #2227, .T. ) ;
#11046 = DIRECTION ( 'NONE',  ( -1.000000000000000000, 0.000000000000000000, 0.000000000000000000 ) ) ;
#11047 = CARTESIAN_POINT ( 'NONE',  ( -0.05175539059627463218, 0.06736074103232447818, 0.07475334604056275978 ) ) ;
#11048 = DIRECTION ( 'NONE',  ( 1.000000000000000000, 0.000000000000000000, 0.000000000000000000 ) ) ;
#11049 = DIRECTION ( 'NONE',  ( 0.8660254037844390407, 0.000000000000000000, -0.4999999999999994449 ) ) ;
#11050 = ADVANCED_FACE ( 'NONE', ( #8528 ), #10186, .F. ) ;
#11051 = DIRECTION ( 'NONE',  ( 0.4999999999999922284, -0.000000000000000000, -0.8660254037844430375 ) ) ;
#11052 = ADVANCED_FACE ( 'NONE', ( #10178 ), #1724, .T. ) ;
#11053 = ORIENTED_EDGE ( 'NONE', *, *, #11335, .F. ) ;
#11054 = ORIENTED_EDGE ( 'NONE', *, *, #13960, .T. ) ;
#11055 = ORIENTED_EDGE ( 'NONE', *, *, #6917, .F. ) ;
#11056 = EDGE_CURVE ( 'NONE', #6453, #2422, #12695, .T. ) ;
#11057 = CARTESIAN_POINT ( 'NONE',  ( 0.1724006475077543565, -0.09842519685039370636, 0.1768186671464649640 ) ) ;
#11058 = CARTESIAN_POINT ( 'NONE',  ( -0.1574803149606299191, -0.003937007874015747977, -0.5909884645248143498 ) ) ;
#11059 = DIRECTION ( 'NONE',  ( 1.000000000000000000, 0.000000000000000000, 0.000000000000000000 ) ) ;
#11060 = CARTESIAN_POINT ( 'NONE',  ( 0.000000000000000000, 0.5590551181102362266, 0.000000000000000000 ) ) ;
#11061 = DIRECTION ( 'NONE',  ( 1.720845688168992638E-15, 0.5695655044020486724, 0.8219459448134287527 ) ) ;
#11062 =( LENGTH_UNIT ( ) NAMED_UNIT ( * ) SI_UNIT ( $, .METRE. ) );
#11063 = CARTESIAN_POINT ( 'NONE',  ( 0.000000000000000000, 0.000000000000000000, 0.000000000000000000 ) ) ;
#11064 = CARTESIAN_POINT ( 'NONE',  ( -0.4307978335858689278, -0.003937007874015747977, 0.4318761856142863120 ) ) ;
#11065 = LINE ( 'NONE', #10450, #13358 ) ;
#11066 = CARTESIAN_POINT ( 'NONE',  ( 0.2686781383420775993, -0.1023622047244094474, 0.03298669471825042832 ) ) ;
#11067 = DIRECTION ( 'NONE',  ( 0.000000000000000000, 4.956352788505160310E-16, 1.000000000000000000 ) ) ;
#11068 = ORIENTED_EDGE ( 'NONE', *, *, #14675, .F. ) ;
#11069 = ORIENTED_EDGE ( 'NONE', *, *, #1370, .T. ) ;
#11070 = AXIS2_PLACEMENT_3D ( 'NONE', #12686, #9157, #9477 ) ;
#11071 = EDGE_LOOP ( 'NONE', ( #1179, #4832 ) ) ;
#11072 = AXIS2_PLACEMENT_3D ( 'NONE', #375, #1250, #6003 ) ;
#11073 = ADVANCED_FACE ( 'NONE', ( #7975 ), #7812, .F. ) ;
#11074 = CIRCLE ( 'NONE', #3596, 0.007874015748031482076 ) ;
#11075 = SHAPE_REPRESENTATION ( 'Connecting Link', ( #11481 ), #10969 ) ;
#11076 = DIRECTION ( 'NONE',  ( -0.000000000000000000, 1.000000000000000000, 0.000000000000000000 ) ) ;
#11077 = CARTESIAN_POINT ( 'NONE',  ( -1.951331694435471498, -2.917526071354513029, 0.07709592686080572743 ) ) ;
#11078 = DIRECTION ( 'NONE',  ( 0.000000000000000000, -1.000000000000000000, -0.000000000000000000 ) ) ;
#11079 = DIRECTION ( 'NONE',  ( 0.000000000000000000, -1.000000000000000000, 0.000000000000000000 ) ) ;
#11080 = DIRECTION ( 'NONE',  ( 0.000000000000000000, 0.000000000000000000, 1.000000000000000000 ) ) ;
#11081 = LINE ( 'NONE', #6063, #12825 ) ;
#11082 = CIRCLE ( 'NONE', #15348, 0.007874015748031504627 ) ;
#11083 = DIRECTION ( 'NONE',  ( 0.000000000000000000, 1.734723475976802677E-14, 1.000000000000000000 ) ) ;
#11084 = CARTESIAN_POINT ( 'NONE',  ( -1.882371321102604078, -2.915739816777954463, 0.04555328826220117477 ) ) ;
#11085 = AXIS2_PLACEMENT_3D ( 'NONE', #135, #2625, #3799 ) ;
#11086 = CARTESIAN_POINT ( 'NONE',  ( 0.000000000000000000, 0.3622047244094487306, 0.000000000000000000 ) ) ;
#11087 = AXIS2_PLACEMENT_3D ( 'NONE', #10054, #1686, #3872 ) ;
#11088 = ORIENTED_EDGE ( 'NONE', *, *, #2538, .T. ) ;
#11089 = ORIENTED_EDGE ( 'NONE', *, *, #14286, .F. ) ;
#11090 = ORIENTED_EDGE ( 'NONE', *, *, #11607, .F. ) ;
#11091 = VERTEX_POINT ( 'NONE', #5614 ) ;
#11092 = VERTEX_POINT ( 'NONE', #13780 ) ;
#11093 = AXIS2_PLACEMENT_3D ( 'NONE', #4742, #210, #13342 ) ;
#11094 = CARTESIAN_POINT ( 'NONE',  ( -1.411972059858401574, -0.03772986244363892711, -0.05403728031753547711 ) ) ;
#11095 = CIRCLE ( 'NONE', #12359, 0.007874015748031501158 ) ;
#11096 = AXIS2_PLACEMENT_3D ( 'NONE', #11435, #7905, #4369 ) ;
#11097 = DIRECTION ( 'NONE',  ( 0.5692328345973367565, 0.000000000000000000, -0.8221763679505029732 ) ) ;
#11098 = VECTOR ( 'NONE', #9685, 39.37007874015748143 ) ;
#11099 = EDGE_CURVE ( 'NONE', #8067, #2107, #15198, .T. ) ;
#11100 = DIRECTION ( 'NONE',  ( -1.000000000000000000, 0.000000000000000000, 0.000000000000000000 ) ) ;
#11101 = DIRECTION ( 'NONE',  ( -0.8660254037844385966, 0.000000000000000000, 0.5000000000000001110 ) ) ;
#11102 = CARTESIAN_POINT ( 'NONE',  ( -2.010991777528384983, -2.758467574604075434, 0.1561691687464110412 ) ) ;
#11103 = CARTESIAN_POINT ( 'NONE',  ( -1.187740243782755556, 0.3305209984255413902, 0.05905511811023626823 ) ) ;
#11104 = CARTESIAN_POINT ( 'NONE',  ( -1.881708026547704860, -2.917360643372564066, -0.03975124946893780070 ) ) ;
#11105 = ORIENTED_EDGE ( 'NONE', *, *, #14570, .F. ) ;
#11106 = CARTESIAN_POINT ( 'NONE',  ( -2.168819294506413087, -1.823050691322769090, -0.1033464566929129108 ) ) ;
#11107 = DIRECTION ( 'NONE',  ( 0.8660254037844385966, 0.000000000000000000, -0.4999999999999998890 ) ) ;
#11108 = CIRCLE ( 'NONE', #7859, 0.007874015748031516770 ) ;
#11109 = CIRCLE ( 'NONE', #15162, 0.003937007874015746242 ) ;
#11110 = AXIS2_PLACEMENT_3D ( 'NONE', #3430, #8205, #5587 ) ;
#11111 = CARTESIAN_POINT ( 'NONE',  ( 6.750021727583836750E-17, 2.393700787401575436, 0.5511811023622046335 ) ) ;
#11112 = VECTOR ( 'NONE', #9083, 39.37007874015748143 ) ;
#11113 = ORIENTED_EDGE ( 'NONE', *, *, #11856, .F. ) ;
#11114 = AXIS2_PLACEMENT_3D ( 'NONE', #3526, #6010, #13 ) ;
#11115 = ORIENTED_EDGE ( 'NONE', *, *, #142, .T. ) ;
#11116 = AXIS2_PLACEMENT_3D ( 'NONE', #2449, #7225, #6025 ) ;
#11117 = CARTESIAN_POINT ( 'NONE',  ( 0.000000000000000000, 1.622047244094488638, 0.5590551181102362266 ) ) ;
#11118 = ORIENTED_EDGE ( 'NONE', *, *, #11623, .F. ) ;
#11119 = EDGE_CURVE ( 'NONE', #1797, #9786, #13935, .T. ) ;
#11120 = CIRCLE ( 'NONE', #12384, 0.04330708661417330407 ) ;
#11121 = VECTOR ( 'NONE', #13814, 39.37007874015748854 ) ;
#11122 = VECTOR ( 'NONE', #5976, 39.37007874015748143 ) ;
#11123 = EDGE_CURVE ( 'NONE', #2263, #12795, #1688, .T. ) ;
#11124 = CYLINDRICAL_SURFACE ( 'NONE', #9878, 0.5905511811023621549 ) ;
#11125 = DIRECTION ( 'NONE',  ( 0.000000000000000000, 0.000000000000000000, 1.000000000000000000 ) ) ;
#11126 = FACE_OUTER_BOUND ( 'NONE', #3264, .T. ) ;
#11127 = CIRCLE ( 'NONE', #15411, 0.007874015748031516770 ) ;
#11128 = CARTESIAN_POINT ( 'NONE',  ( -0.02281238468002976319, -0.1806356120156163148, -0.007039490205851098130 ) ) ;
#11129 = ORIENTED_EDGE ( 'NONE', *, *, #11461, .F. ) ;
#11130 = CARTESIAN_POINT ( 'NONE',  ( -0.3706061991976995484, -0.09842519685039370636, -0.2139695888701363957 ) ) ;
#11131 = SPHERICAL_SURFACE ( 'NONE', #4334, 0.01968503937007873988 ) ;
#11132 = DIRECTION ( 'NONE',  ( 0.000000000000000000, 0.000000000000000000, -1.000000000000000000 ) ) ;
#11133 = LINE ( 'NONE', #13796, #8705 ) ;
#11134 = CARTESIAN_POINT ( 'NONE',  ( 0.04921259842519617317, -0.4881889763779528324, 0.08523872084492387091 ) ) ;
#11135 = VECTOR ( 'NONE', #4692, 39.37007874015748143 ) ;
#11136 = CIRCLE ( 'NONE', #11909, 0.1240157480314959260 ) ;
#11137 = AXIS2_PLACEMENT_3D ( 'NONE', #10462, #14293, #9525 ) ;
#11138 = ORIENTED_EDGE ( 'NONE', *, *, #10559, .T. ) ;
#11139 = ORIENTED_EDGE ( 'NONE', *, *, #2369, .T. ) ;
#11140 = EDGE_CURVE ( 'NONE', #7200, #1180, #7900, .T. ) ;
#11141 = EDGE_LOOP ( 'NONE', ( #13821, #7136, #12906, #10533 ) ) ;
#11142 = PLANE ( 'NONE',  #653 ) ;
#11143 = FACE_BOUND ( 'NONE', #1444, .T. ) ;
#11144 = ADVANCED_FACE ( 'NONE', ( #5528 ), #12532, .T. ) ;
#11145 = CARTESIAN_POINT ( 'NONE',  ( -0.04921259842519618705, -0.4881889763779528324, 0.08523872084492388479 ) ) ;
#11146 = CARTESIAN_POINT ( 'NONE',  ( -0.1552072824047653066, -0.09842519685039370636, -0.5870514566507987197 ) ) ;
#11147 = DIRECTION ( 'NONE',  ( -0.2084205441254115276, 0.9706086590632821975, -0.1203316572554556929 ) ) ;
#11148 = AXIS2_PLACEMENT_3D ( 'NONE', #14761, #7702, #340 ) ;
#11149 = CARTESIAN_POINT ( 'NONE',  ( -1.403610094870331393, -0.004984718095728941228, 0.05942212872828700476 ) ) ;
#11150 = AXIS2_PLACEMENT_3D ( 'NONE', #11254, #5362, #14859 ) ;
#11151 = CARTESIAN_POINT ( 'NONE',  ( -0.1062992125983148878, -0.1023622047244094474, -0.5870514566507987197 ) ) ;
#11152 = VECTOR ( 'NONE', #9759, 39.37007874015748143 ) ;
#11153 = CARTESIAN_POINT ( 'NONE',  ( 0.2661821753648509481, -0.4881889763779528324, 0.03548265769547701703 ) ) ;
#11154 = FACE_BOUND ( 'NONE', #12656, .T. ) ;
#11155 = CARTESIAN_POINT ( 'NONE',  ( 0.000000000000000000, -0.09842519685039370636, 0.000000000000000000 ) ) ;
#11156 = VECTOR ( 'NONE', #14517, 39.37007874015748143 ) ;
#11157 = DIRECTION ( 'NONE',  ( 0.000000000000000000, 0.000000000000000000, 1.000000000000000000 ) ) ;
#11158 = EDGE_LOOP ( 'NONE', ( #5228, #9604, #13716, #11326 ) ) ;
#11159 = ORIENTED_EDGE ( 'NONE', *, *, #1538, .F. ) ;
#11160 = ORIENTED_EDGE ( 'NONE', *, *, #10665, .T. ) ;
#11161 = CIRCLE ( 'NONE', #6396, 0.03937007874015751446 ) ;
#11162 = ORIENTED_EDGE ( 'NONE', *, *, #10199, .T. ) ;
#11163 = AXIS2_PLACEMENT_3D ( 'NONE', #13731, #6654, #6497 ) ;
#11164 = ADVANCED_BREP_SHAPE_REPRESENTATION ( '', ( #14611, #11481 ), #10969 ) ;
#11165 = FACE_OUTER_BOUND ( 'NONE', #13196, .T. ) ;
#11166 = CARTESIAN_POINT ( 'NONE',  ( -1.938752474876189069, -2.948113922056589065, -0.02541044617147641266 ) ) ;
#11167 =( NAMED_UNIT ( * ) SI_UNIT ( $, .STERADIAN. ) SOLID_ANGLE_UNIT ( ) );
#11168 = EDGE_CURVE ( 'NONE', #6389, #14049, #12603, .T. ) ;
#11169 = CARTESIAN_POINT ( 'NONE',  ( -1.180847381051866485, 0.3433074774306730803, -0.03937007874015747977 ) ) ;
#11170 = CARTESIAN_POINT ( 'NONE',  ( -1.995574481745110651, -2.802154287413662459, -0.1558670771739966432 ) ) ;
#11171 = DIRECTION ( 'NONE',  ( 0.000000000000000000, 0.000000000000000000, 1.000000000000000000 ) ) ;
#11172 = DIRECTION ( 'NONE',  ( -0.000000000000000000, -0.000000000000000000, -1.000000000000000000 ) ) ;
#11173 = EDGE_CURVE ( 'NONE', #6881, #4497, #11269, .T. ) ;
#11174 = CARTESIAN_POINT ( 'NONE',  ( -0.3441669734936866343, 2.010494531933507467, -0.05905511811023622659 ) ) ;
#11175 = EDGE_CURVE ( 'NONE', #4716, #10501, #8838, .T. ) ;
#11176 = DIRECTION ( 'NONE',  ( -0.4999999999999979461, 0.000000000000000000, -0.8660254037844398178 ) ) ;
#11177 = CARTESIAN_POINT ( 'NONE',  ( 0.000000000000000000, 0.000000000000000000, 0.000000000000000000 ) ) ;
#11178 = ORIENTED_EDGE ( 'NONE', *, *, #9270, .T. ) ;
#11179 = ORIENTED_EDGE ( 'NONE', *, *, #15185, .T. ) ;
#11180 = VECTOR ( 'NONE', #8012, 39.37007874015748854 ) ;
#11181 = ORIENTED_EDGE ( 'NONE', *, *, #15301, .T. ) ;
#11182 = ORIENTED_EDGE ( 'NONE', *, *, #14203, .F. ) ;
#11183 = VECTOR ( 'NONE', #9793, 39.37007874015748143 ) ;
#11184 = ORIENTED_EDGE ( 'NONE', *, *, #3831, .F. ) ;
#11185 = CIRCLE ( 'NONE', #5164, 0.04330708661417324162 ) ;
#11186 = DIRECTION ( 'NONE',  ( 0.8660254037844387076, 0.000000000000000000, 0.5000000000000001110 ) ) ;
#11187 = DIRECTION ( 'NONE',  ( 1.000000000000000000, 0.000000000000000000, 0.000000000000000000 ) ) ;
#11188 = AXIS2_PLACEMENT_3D ( 'NONE', #10641, #9627, #14548 ) ;
#11189 = DIRECTION ( 'NONE',  ( 0.000000000000000000, -1.000000000000000000, 0.000000000000000000 ) ) ;
#11190 = PRODUCT_DEFINITION_SHAPE ( 'NONE', 'NONE',  #15491 ) ;
#11191 = CARTESIAN_POINT ( 'NONE',  ( -0.06692913385815735250, -0.4921259842519685179, -0.5909884645248143498 ) ) ;
#11192 = DIRECTION ( 'NONE',  ( 1.000000000000000000, 0.000000000000000000, 0.000000000000000000 ) ) ;
#11193 = VECTOR ( 'NONE', #14279, 39.37007874015748143 ) ;
#11194 = CARTESIAN_POINT ( 'NONE',  ( -0.4307978335858689833, -0.003937007874015747977, 0.4279391777402706265 ) ) ;
#11195 = CARTESIAN_POINT ( 'NONE',  ( -0.4765664223158451174, 1.344138844425170731, 0.3487699017373184218 ) ) ;
#11196 = CARTESIAN_POINT ( 'NONE',  ( -1.875101537351226311, -2.933668943012675001, 0.07363248663697015417 ) ) ;
#11197 = ORIENTED_EDGE ( 'NONE', *, *, #10779, .T. ) ;
#11198 = DIRECTION ( 'NONE',  ( 0.000000000000000000, 1.000000000000000000, 0.000000000000000000 ) ) ;
#11199 = EDGE_CURVE ( 'NONE', #10309, #10256, #5956, .T. ) ;
#11200 = AXIS2_PLACEMENT_3D ( 'NONE', #11589, #862, #14024 ) ;
#11201 = AXIS2_PLACEMENT_3D ( 'NONE', #2070, #14814, #493 ) ;
#11202 = CARTESIAN_POINT ( 'NONE',  ( -1.416791279958480976, -0.01064335357298143957, -0.06799382560225487870 ) ) ;
#11203 = ORIENTED_EDGE ( 'NONE', *, *, #8631, .T. ) ;
#11204 = ORIENTED_EDGE ( 'NONE', *, *, #8008, .T. ) ;
#11205 = CIRCLE ( 'NONE', #7951, 0.007874015748031449116 ) ;
#11206 = ORIENTED_EDGE ( 'NONE', *, *, #13102, .T. ) ;
#11207 = AXIS2_PLACEMENT_3D ( 'NONE', #12843, #6494, #12620 ) ;
#11208 = DIRECTION ( 'NONE',  ( -0.8660254037844363761, 0.000000000000000000, 0.5000000000000038858 ) ) ;
#11209 = LINE ( 'NONE', #7121, #6109 ) ;
#11210 = AXIS2_PLACEMENT_3D ( 'NONE', #6285, #13220, #7258 ) ;
#11211 = CARTESIAN_POINT ( 'NONE',  ( 0.06692913385832209572, -0.4881889763779528324, -0.2377126739437405434 ) ) ;
#11212 = CARTESIAN_POINT ( 'NONE',  ( 0.06299212598430639631, -0.4881889763779528324, -0.5870514566507987197 ) ) ;
#11213 = ORIENTED_EDGE ( 'NONE', *, *, #5192, .T. ) ;
#11214 = EDGE_CURVE ( 'NONE', #777, #2454, #4284, .T. ) ;
#11215 = FACE_OUTER_BOUND ( 'NONE', #7316, .T. ) ;
#11216 = CARTESIAN_POINT ( 'NONE',  ( -0.5905511811023629321, -0.09448818897637796532, 0.1591122789105256785 ) ) ;
#11217 = CYLINDRICAL_SURFACE ( 'NONE', #2146, 0.003937007874015749712 ) ;
#11218 = DIRECTION ( 'NONE',  ( 0.000000000000000000, 1.000000000000000000, 0.000000000000000000 ) ) ;
#11219 = ADVANCED_FACE ( 'NONE', ( #9073 ), #571, .T. ) ;
#11220 = DIRECTION ( 'NONE',  ( 0.000000000000000000, 1.000000000000000000, 0.000000000000000000 ) ) ;
#11221 = FILL_AREA_STYLE_COLOUR ( '', #11424 ) ;
#11222 = AXIS2_PLACEMENT_3D ( 'NONE', #12002, #9412, #13074 ) ;
#11223 = ORIENTED_EDGE ( 'NONE', *, *, #14866, .F. ) ;
#11224 = EDGE_CURVE ( 'NONE', #4333, #7634, #4573, .T. ) ;
#11225 = EDGE_LOOP ( 'NONE', ( #7037, #13085, #1628, #10708 ) ) ;
#11226 = VERTEX_POINT ( 'NONE', #15334 ) ;
#11227 = FACE_OUTER_BOUND ( 'NONE', #8051, .T. ) ;
#11228 = CARTESIAN_POINT ( 'NONE',  ( -0.3623183339751723242, -0.2952755905511811330, 0.1319014807535664191 ) ) ;
#11229 = B_SPLINE_CURVE_WITH_KNOTS ( 'NONE', 3,
 ( #5500, #3008, #6588, #13813, #10222, #14835 ),
 .UNSPECIFIED., .F., .F.,
 ( 4, 2, 4 ),
 ( 0.002383301291214095802, 0.01571728647480164637, 0.02905127165838919390 ),
 .UNSPECIFIED. ) ;
#11230 = CARTESIAN_POINT ( 'NONE',  ( -1.960442862720704005, -2.701045185997201781, 0.1503165316663955531 ) ) ;
#11231 = DIRECTION ( 'NONE',  ( 0.000000000000000000, 0.000000000000000000, -1.000000000000000000 ) ) ;
#11232 = APPLICATION_PROTOCOL_DEFINITION ( 'draft international standard', 'automotive_design', 1998, #7790 ) ;
#11233 = LINE ( 'NONE', #4252, #2620 ) ;
#11234 = ADVANCED_FACE ( 'NONE', ( #3514 ), #11901, .T. ) ;
#11235 = CARTESIAN_POINT ( 'NONE',  ( 0.6864776960422567242, 1.338582677165354395, 0.4645290592786021633 ) ) ;
#11236 = FACE_OUTER_BOUND ( 'NONE', #2328, .T. ) ;
#11237 = EDGE_CURVE ( 'NONE', #8301, #3987, #14077, .T. ) ;
#11238 = CARTESIAN_POINT ( 'NONE',  ( -1.992382107315058271, -2.752050336136262931, 0.1561691687464115408 ) ) ;
#11239 = VERTEX_POINT ( 'NONE', #4597 ) ;
#11240 = VERTEX_POINT ( 'NONE', #5836 ) ;
#11241 = ADVANCED_FACE ( 'NONE', ( #15425 ), #8573, .F. ) ;
#11242 = ORIENTED_EDGE ( 'NONE', *, *, #15218, .F. ) ;
#11243 = VERTEX_POINT ( 'NONE', #10487 ) ;
#11244 = CARTESIAN_POINT ( 'NONE',  ( 0.1028896637646825596, -0.4881889763779528324, -0.2462933508111075365 ) ) ;
#11245 = CARTESIAN_POINT ( 'NONE',  ( -1.927778962255358053, -2.941963733592956487, -0.05151121078832996553 ) ) ;
#11246 =( CONVERSION_BASED_UNIT ( 'INCH', #6460 ) LENGTH_UNIT ( ) NAMED_UNIT ( #15269 ) );
#11247 = DIRECTION ( 'NONE',  ( 1.000000000000000000, 0.000000000000000000, 0.000000000000000000 ) ) ;
#11248 = CARTESIAN_POINT ( 'NONE',  ( -1.984789438093313541, -2.774065754419840601, -0.1775759736344397766 ) ) ;
#11249 = DIRECTION ( 'NONE',  ( 0.000000000000000000, 0.000000000000000000, -1.000000000000000000 ) ) ;
#11250 = DIRECTION ( 'NONE',  ( 0.000000000000000000, 0.000000000000000000, 1.000000000000000000 ) ) ;
#11251 = ADVANCED_FACE ( 'NONE', ( #10718 ), #11751, .F. ) ;
#11252 = CARTESIAN_POINT ( 'NONE',  ( -1.884728029847772879, -2.909954979002622011, 0.06162763431411907855 ) ) ;
#11253 = DIRECTION ( 'NONE',  ( 0.000000000000000000, 1.000000000000000000, 0.000000000000000000 ) ) ;
#11254 = CARTESIAN_POINT ( 'NONE',  ( 0.000000000000000000, 0.000000000000000000, 0.000000000000000000 ) ) ;
#11255 = ORIENTED_EDGE ( 'NONE', *, *, #14195, .T. ) ;
#11256 = ORIENTED_EDGE ( 'NONE', *, *, #9551, .T. ) ;
#11257 = ADVANCED_FACE ( 'NONE', ( #8357 ), #4066, .T. ) ;
#11258 = ORIENTED_EDGE ( 'NONE', *, *, #9429, .F. ) ;
#11259 = ORIENTED_EDGE ( 'NONE', *, *, #10347, .F. ) ;
#11260 = ORIENTED_EDGE ( 'NONE', *, *, #13152, .F. ) ;
#11261 = CARTESIAN_POINT ( 'NONE',  ( -1.389961391698828708, -0.02151349750585865306, -0.06002070848877767706 ) ) ;
#11262 = ADVANCED_FACE ( 'NONE', ( #10786 ), #4760, .F. ) ;
#11263 = CARTESIAN_POINT ( 'NONE',  ( 0.05823215749475442460, 0.06963377358823460983, -0.06105365336398921317 ) ) ;
#11264 = DIRECTION ( 'NONE',  ( -0.5000000000000059952, 0.000000000000000000, 0.8660254037844351549 ) ) ;
#11265 = CARTESIAN_POINT ( 'NONE',  ( -2.111626822439223172, -2.421545435136619684, 0.1175637245596499597 ) ) ;
#11266 = CARTESIAN_POINT ( 'NONE',  ( 0.000000000000000000, 0.1692468441617604180, -0.03937007874015747977 ) ) ;
#11267 = FACE_OUTER_BOUND ( 'NONE', #6118, .T. ) ;
#11268 = CARTESIAN_POINT ( 'NONE',  ( -1.141732283464566677, 4.821444091131322309E-18, 0.02559055118110236185 ) ) ;
#11269 = LINE ( 'NONE', #12759, #9227 ) ;
#11270 = CARTESIAN_POINT ( 'NONE',  ( -1.908239321022362489, -2.920800340391614291, -0.09749645815890824185 ) ) ;
#11271 = EDGE_LOOP ( 'NONE', ( #1346, #3243, #7630, #4170 ) ) ;
#11272 = CARTESIAN_POINT ( 'NONE',  ( -2.163017314575554462, -1.630597114118274238, -0.1033464566929129386 ) ) ;
#11273 = LINE ( 'NONE', #8845, #5950 ) ;
#11274 = ORIENTED_EDGE ( 'NONE', *, *, #4229, .T. ) ;
#11275 = ORIENTED_EDGE ( 'NONE', *, *, #1501, .T. ) ;
#11276 = UNCERTAINTY_MEASURE_WITH_UNIT (LENGTH_MEASURE( 1.000000000000000082E-05 ), #11246, 'distance_accuracy_value', 'NONE');
#11277 = VERTEX_POINT ( 'NONE', #5924 ) ;
#11278 = EDGE_CURVE ( 'NONE', #7659, #4124, #4316, .T. ) ;
#11279 = CYLINDRICAL_SURFACE ( 'NONE', #5833, 0.01968503937007875723 ) ;
#11280 = LINE ( 'NONE', #14813, #13209 ) ;
#11281 = CARTESIAN_POINT ( 'NONE',  ( 0.000000000000000000, 0.000000000000000000, 0.000000000000000000 ) ) ;
#11282 = CARTESIAN_POINT ( 'NONE',  ( -0.06997480235680504645, -0.1674783595965826377, -0.05905511811023622659 ) ) ;
#11283 = VERTEX_POINT ( 'NONE', #3272 ) ;
#11284 = DIRECTION ( 'NONE',  ( 0.000000000000000000, 1.000000000000000000, 0.000000000000000000 ) ) ;
#11285 = PLANE ( 'NONE',  #3862 ) ;
#11286 = DIRECTION ( 'NONE',  ( 0.000000000000000000, -1.000000000000000000, 0.000000000000000000 ) ) ;
#11287 = CARTESIAN_POINT ( 'NONE',  ( -0.1552072824047652788, -0.003937007874015747977, -0.5870514566507987197 ) ) ;
#11288 = ORIENTED_EDGE ( 'NONE', *, *, #5315, .F. ) ;
#11289 = ORIENTED_EDGE ( 'NONE', *, *, #13764, .F. ) ;
#11290 = EDGE_LOOP ( 'NONE', ( #1557, #4589, #1288, #8244 ) ) ;
#11291 = APPLICATION_CONTEXT ( 'automotive_design' ) ;
#11292 = DIRECTION ( 'NONE',  ( -0.000000000000000000, -1.000000000000000000, -0.000000000000000000 ) ) ;
#11293 = CARTESIAN_POINT ( 'NONE',  ( -0.07500546397816693078, 0.1646499958011362896, -0.03937007824588655003 ) ) ;
#11294 = CARTESIAN_POINT ( 'NONE',  ( -0.06299212598414161146, -0.1023622047244094474, -0.5909884645248154600 ) ) ;
#11295 =( NAMED_UNIT ( * ) SI_UNIT ( $, .STERADIAN. ) SOLID_ANGLE_UNIT ( ) );
#11296 = DIRECTION ( 'NONE',  ( 0.000000000000000000, 0.000000000000000000, -1.000000000000000000 ) ) ;
#11297 = CARTESIAN_POINT ( 'NONE',  ( -0.1062992125983148878, -0.1023622047244094474, -0.5870514566507987197 ) ) ;
#11298 = DIRECTION ( 'NONE',  ( 0.4999999999999798495, 0.000000000000000000, -0.8660254037844501429 ) ) ;
#11299 = EDGE_CURVE ( 'NONE', #2422, #14454, #13083, .T. ) ;
#11300 = CARTESIAN_POINT ( 'NONE',  ( 0.000000000000000000, 1.346456692913385877, -0.5984251968503937480 ) ) ;
#11301 = DIRECTION ( 'NONE',  ( -1.000000000000000000, 0.000000000000000000, 0.000000000000000000 ) ) ;
#11302 = ORIENTED_EDGE ( 'NONE', *, *, #10590, .T. ) ;
#11303 = EDGE_LOOP ( 'NONE', ( #4853, #9505, #11979, #11547 ) ) ;
#11304 = VERTEX_POINT ( 'NONE', #4454 ) ;
#11305 = VERTEX_POINT ( 'NONE', #9237 ) ;
#11306 = ADVANCED_FACE ( 'NONE', ( #6871 ), #9836, .F. ) ;
#11307 = EDGE_CURVE ( 'NONE', #12795, #2263, #12084, .T. ) ;
#11308 = DIRECTION ( 'NONE',  ( 0.4999999999999966693, 0.000000000000000000, 0.8660254037844405950 ) ) ;
#11309 = CARTESIAN_POINT ( 'NONE',  ( -1.954244229570128111, -2.867204336101874418, 0.1501281538326428022 ) ) ;
#11310 =( LENGTH_UNIT ( ) NAMED_UNIT ( * ) SI_UNIT ( $, .METRE. ) );
#11311 = CARTESIAN_POINT ( 'NONE',  ( 0.000000000000000000, 0.5984251968503937480, -0.5905511811023621549 ) ) ;
#11312 = EDGE_CURVE ( 'NONE', #4031, #13771, #1819, .T. ) ;
#11313 = CARTESIAN_POINT ( 'NONE',  ( -2.010991777528384095, -2.758467574604078543, -0.1561691687464109024 ) ) ;
#11314 = CARTESIAN_POINT ( 'NONE',  ( 0.000000000000000000, 0.3543307086614172485, -0.6614173228346456046 ) ) ;
#11315 = DIRECTION ( 'NONE',  ( 0.000000000000000000, -0.000000000000000000, 1.000000000000000000 ) ) ;
#11316 = CARTESIAN_POINT ( 'NONE',  ( -1.883711820814927274, -2.912463908419459901, -0.05618017532687354099 ) ) ;
#11317 = CARTESIAN_POINT ( 'NONE',  ( 0.000000000000000000, 0.4094488188976377896, 0.000000000000000000 ) ) ;
#11318 = CARTESIAN_POINT ( 'NONE',  ( -2.090218168050184122, -1.822025907981831727, -0.08562854774378582390 ) ) ;
#11319 = AXIS2_PLACEMENT_3D ( 'NONE', #1312, #153, #4913 ) ;
#11320 = ORIENTED_EDGE ( 'NONE', *, *, #11434, .T. ) ;
#11321 = AXIS2_PLACEMENT_3D ( 'NONE', #2416, #7194, #2783 ) ;
#11322 = ORIENTED_EDGE ( 'NONE', *, *, #1785, .T. ) ;
#11323 = ORIENTED_EDGE ( 'NONE', *, *, #3019, .T. ) ;
#11324 = VERTEX_POINT ( 'NONE', #14010 ) ;
#11325 = EDGE_CURVE ( 'NONE', #12382, #7799, #2562, .T. ) ;
#11326 = ORIENTED_EDGE ( 'NONE', *, *, #8473, .F. ) ;
#11327 = ADVANCED_FACE ( 'NONE', ( #12994 ), #5760, .T. ) ;
#11328 = CARTESIAN_POINT ( 'NONE',  ( 0.5615510810874363434, -0.1023622047244094474, 0.2014679098129276147 ) ) ;
#11329 = DIRECTION ( 'NONE',  ( 0.4999999999999979461, 0.000000000000000000, 0.8660254037844398178 ) ) ;
#11330 = TOROIDAL_SURFACE ( 'NONE', #11853, 0.1614173228346456879, 0.003937007874015747977 ) ;
#11331 = VECTOR ( 'NONE', #11640, 39.37007874015748143 ) ;
#11332 = CARTESIAN_POINT ( 'NONE',  ( 0.04921259842519613847, -0.4921259842519685179, 0.08523872084492380152 ) ) ;
#11333 = AXIS2_PLACEMENT_3D ( 'NONE', #15129, #9257, #9096 ) ;
#11334 = DIRECTION ( 'NONE',  ( -0.000000000000000000, 1.000000000000000000, 0.000000000000000000 ) ) ;
#11335 = EDGE_CURVE ( 'NONE', #10948, #9186, #11081, .T. ) ;
#11336 = CARTESIAN_POINT ( 'NONE',  ( 0.4749369078591172411, -0.1023622047244094474, 0.3514880584999470203 ) ) ;
#11337 = AXIS2_PLACEMENT_3D ( 'NONE', #14965, #9007, #12368 ) ;
#11338 = EDGE_CURVE ( 'NONE', #10031, #13899, #8831, .T. ) ;
#11339 = DIRECTION ( 'NONE',  ( 0.000000000000000000, 0.000000000000000000, 1.000000000000000000 ) ) ;
#11340 = DIRECTION ( 'NONE',  ( -0.000000000000000000, -1.000000000000000000, 0.000000000000000000 ) ) ;
#11341 = CARTESIAN_POINT ( 'NONE',  ( -1.945459748359985142, -2.745801194614594376, -0.1561691687464109302 ) ) ;
#11342 = ORIENTED_EDGE ( 'NONE', *, *, #4945, .F. ) ;
#11343 = CARTESIAN_POINT ( 'NONE',  ( 0.05905511811023622659, 1.190944881889763884, -0.8267716535433072833 ) ) ;
#11344 = B_SPLINE_CURVE_WITH_KNOTS ( 'NONE', 3,
 ( #10302, #7793, #6611, #11409, #5589 ),
 .UNSPECIFIED., .F., .F.,
 ( 4, 1, 4 ),
 ( 2.432568093614346639E-07, 0.001154943795188590611, 0.002309644333567820521 ),
 .UNSPECIFIED. ) ;
#11345 = CARTESIAN_POINT ( 'NONE',  ( -1.596030944582063960, 0.1136756404979307328, 0.04477369844320258641 ) ) ;
#11346 = ORIENTED_EDGE ( 'NONE', *, *, #2182, .T. ) ;
#11347 = EDGE_CURVE ( 'NONE', #13444, #15235, #8819, .T. ) ;
#11348 = ORIENTED_EDGE ( 'NONE', *, *, #3447, .F. ) ;
#11349 = CIRCLE ( 'NONE', #14103, 0.003937007874015724558 ) ;
#11350 = VECTOR ( 'NONE', #9338, 39.37007874015748143 ) ;
#11351 = CIRCLE ( 'NONE', #6332, 0.1535433070866141780 ) ;
#11352 = VECTOR ( 'NONE', #2992, 39.37007874015748143 ) ;
#11353 = ORIENTED_EDGE ( 'NONE', *, *, #12633, .T. ) ;
#11354 = CARTESIAN_POINT ( 'NONE',  ( -0.5084014747882513729, -0.09842519685039370636, 0.2935257283253980831 ) ) ;
#11355 = EDGE_CURVE ( 'NONE', #14453, #12673, #7821, .T. ) ;
#11356 = CARTESIAN_POINT ( 'NONE',  ( -0.5905511811023629321, -0.003937007874015747977, 0.1591122789105256785 ) ) ;
#11357 = VECTOR ( 'NONE', #4805, 39.37007874015748143 ) ;
#11358 = DIRECTION ( 'NONE',  ( -0.000000000000000000, 0.000000000000000000, 1.000000000000000000 ) ) ;
#11359 = CIRCLE ( 'NONE', #12621, 0.003937007874015747977 ) ;
#11360 = LINE ( 'NONE', #12546, #10141 ) ;
#11361 = ORIENTED_EDGE ( 'NONE', *, *, #1196, .T. ) ;
#11362 = DIRECTION ( 'NONE',  ( 0.5000000000000008882, -0.000000000000000000, -0.8660254037844380415 ) ) ;
#11363 = CIRCLE ( 'NONE', #14383, 0.2303149606299203511 ) ;
#11364 = CARTESIAN_POINT ( 'NONE',  ( 0.000000000000000000, 1.035433070866142335, 0.000000000000000000 ) ) ;
#11365 = AXIS2_PLACEMENT_3D ( 'NONE', #14659, #4938, #12156 ) ;
#11366 = AXIS2_PLACEMENT_3D ( 'NONE', #2837, #1591, #7618 ) ;
#11367 = CARTESIAN_POINT ( 'NONE',  ( -0.02015118043373552090, -0.1802412052441877965, 0.0009776059035733464502 ) ) ;
#11368 = EDGE_CURVE ( 'NONE', #12169, #14199, #2640, .T. ) ;
#11369 = DIRECTION ( 'NONE',  ( 1.000000000000000000, -1.813574543066661640E-15, 0.000000000000000000 ) ) ;
#11370 = AXIS2_PLACEMENT_3D ( 'NONE', #13117, #4802, #2698 ) ;
#11371 = EDGE_CURVE ( 'NONE', #115, #15219, #2721, .T. ) ;
#11372 = CARTESIAN_POINT ( 'NONE',  ( -1.180847381051866485, 0.3433074774306730803, -0.03937007874015747977 ) ) ;
#11373 = EDGE_LOOP ( 'NONE', ( #14308, #13027, #6261, #10011, #9380, #11675 ) ) ;
#11375 = ORIENTED_EDGE ( 'NONE', *, *, #39, .T. ) ;
#11374 = CIRCLE ( 'NONE', #4619, 0.007874015748031482076 ) ;
#11376 = AXIS2_PLACEMENT_3D ( 'NONE', #10246, #12682, #15029 ) ;
#11377 = ORIENTED_EDGE ( 'NONE', *, *, #6942, .F. ) ;
#11378 = VECTOR ( 'NONE', #13181, 39.37007874015748143 ) ;
#11379 = CARTESIAN_POINT ( 'NONE',  ( -0.1618514667033795484, -0.1023622047244094474, 0.2161887458866224576 ) ) ;
#11380 = DIRECTION ( 'NONE',  ( -0.000000000000000000, -1.000000000000000000, -0.000000000000000000 ) ) ;
#11381 = AXIS2_PLACEMENT_3D ( 'NONE', #13485, #8626, #2749 ) ;
#11382 = CARTESIAN_POINT ( 'NONE',  ( -2.042401582839019181, -2.380935903742845028, 0.1158648208881124103 ) ) ;
#11383 = DIRECTION ( 'NONE',  ( -0.000000000000000000, -0.000000000000000000, -1.000000000000000000 ) ) ;
#11384 = DIRECTION ( 'NONE',  ( -0.7279172371609822223, 0.5417705490259634438, -0.4202632128226648778 ) ) ;
#11385 = CARTESIAN_POINT ( 'NONE',  ( 0.03450359373084972703, 0.06995722947081550736, -0.07617071561662594470 ) ) ;
#11386 = DIRECTION ( 'NONE',  ( 0.000000000000000000, 0.000000000000000000, -1.000000000000000000 ) ) ;
#11387 = ORIENTED_EDGE ( 'NONE', *, *, #6178, .T. ) ;
#11388 = CARTESIAN_POINT ( 'NONE',  ( -1.078976767140036319, 0.8059172436903675463, -0.03937007874015747977 ) ) ;
#11389 = CARTESIAN_POINT ( 'NONE',  ( 0.1763376553817700698, -0.1023622047244094474, 0.1699995694788709322 ) ) ;
#11390 = CARTESIAN_POINT ( 'NONE',  ( 4.821444091131316146E-18, 0.07874015748031495954, 0.03937007874015751446 ) ) ;
#11391 = AXIS2_PLACEMENT_3D ( 'NONE', #6800, #3289, #9021 ) ;
#11392 = AXIS2_PLACEMENT_3D ( 'NONE', #14320, #940, #10723 ) ;
#11393 = AXIS2_PLACEMENT_3D ( 'NONE', #8827, #11186, #1717 ) ;
#11394 = LINE ( 'NONE', #1828, #6154 ) ;
#11395 = TOROIDAL_SURFACE ( 'NONE', #2379, 0.04330708661417328326, 0.003937007874015747977 ) ;
#11396 = ORIENTED_EDGE ( 'NONE', *, *, #6917, .T. ) ;
#11397 = CARTESIAN_POINT ( 'NONE',  ( 0.000000000000000000, 0.3622047244094487306, -0.6614173228346456046 ) ) ;
#11398 = ORIENTED_EDGE ( 'NONE', *, *, #8287, .F. ) ;
#11399 = ORIENTED_EDGE ( 'NONE', *, *, #15011, .F. ) ;
#11400 = AXIS2_PLACEMENT_3D ( 'NONE', #8990, #4270, #4120 ) ;
#11401 = AXIS2_PLACEMENT_3D ( 'NONE', #15022, #1709, #7962 ) ;
#11402 = VECTOR ( 'NONE', #14258, 39.37007874015748143 ) ;
#11403 = DIRECTION ( 'NONE',  ( 0.000000000000000000, 0.000000000000000000, 1.000000000000000000 ) ) ;
#11404 = CARTESIAN_POINT ( 'NONE',  ( -1.997525977910308947, -2.796737313284686000, 0.1565702274318891973 ) ) ;
#11405 = AXIS2_PLACEMENT_3D ( 'NONE', #10942, #10785, #11900 ) ;
#11406 = CARTESIAN_POINT ( 'NONE',  ( -1.181102362204724310, 0.000000000000000000, -0.02952755905511811330 ) ) ;
#11407 = CARTESIAN_POINT ( 'NONE',  ( -1.994705048877226661, -2.804564119885714302, -0.1744288896405255807 ) ) ;
#11408 = DIRECTION ( 'NONE',  ( 0.000000000000000000, 0.000000000000000000, 1.000000000000000000 ) ) ;
#11409 = CARTESIAN_POINT ( 'NONE',  ( 0.04748649982359187671, 0.06963377358818940988, 0.06973926505267954989 ) ) ;
#11410 = ADVANCED_FACE ( 'NONE', ( #294 ), #9587, .T. ) ;
#11411 = CARTESIAN_POINT ( 'NONE',  ( -0.5595825771504281398, -0.1023622047244094474, 0.2048774586467239645 ) ) ;
#11412 = DIRECTION ( 'NONE',  ( -0.000000000000000000, 1.000000000000000000, 0.000000000000000000 ) ) ;
#11413 = AXIS2_PLACEMENT_3D ( 'NONE', #13805, #3067, #7843 ) ;
#11414 = ADVANCED_FACE ( 'NONE', ( #8582 ), #7318, .F. ) ;
#11415 = ORIENTED_EDGE ( 'NONE', *, *, #9928, .T. ) ;
#11416 = ORIENTED_EDGE ( 'NONE', *, *, #5038, .T. ) ;
#11417 = VERTEX_POINT ( 'NONE', #4822 ) ;
#11418 = AXIS2_PLACEMENT_3D ( 'NONE', #14447, #11046, #1213 ) ;
#11419 = ORIENTED_EDGE ( 'NONE', *, *, #2369, .F. ) ;
#11420 = EDGE_CURVE ( 'NONE', #1499, #8246, #2549, .T. ) ;
#11421 = DIRECTION ( 'NONE',  ( 0.5000000000000014433, -0.000000000000000000, -0.8660254037844378194 ) ) ;
#11422 = CARTESIAN_POINT ( 'NONE',  ( 0.03886060139087953863, 0.06736074103232488064, 0.08219815605943972536 ) ) ;
#11423 = FACE_BOUND ( 'NONE', #11071, .T. ) ;
#11424 = COLOUR_RGB ( '',0.7921568627450980005, 0.8196078431372548767, 0.9333333333333333481 ) ;
#11425 = CARTESIAN_POINT ( 'NONE',  ( 1.181102362204724310, 4.044111181948214319E-16, 0.02559055118110236185 ) ) ;
#11426 = CARTESIAN_POINT ( 'NONE',  ( 0.000000000000000000, 1.377952755905512028, 0.000000000000000000 ) ) ;
#11427 = DIRECTION ( 'NONE',  ( 0.000000000000000000, 0.000000000000000000, -1.000000000000000000 ) ) ;
#11428 = DIRECTION ( 'NONE',  ( -0.000000000000000000, -1.000000000000000000, -0.000000000000000000 ) ) ;
#11429 = DIRECTION ( 'NONE',  ( 0.000000000000000000, 0.000000000000000000, -1.000000000000000000 ) ) ;
#11430 = CIRCLE ( 'NONE', #12687, 0.003937007874015743640 ) ;
#11431 = CARTESIAN_POINT ( 'NONE',  ( -1.915562887302063144, -2.830608845893845871, -0.1438018468321328736 ) ) ;
#11432 = VERTEX_POINT ( 'NONE', #6288 ) ;
#11433 = CARTESIAN_POINT ( 'NONE',  ( -0.3441669734936866343, 2.010494531933507467, -0.03937007874015747977 ) ) ;
#11434 = EDGE_CURVE ( 'NONE', #4524, #9377, #2820, .T. ) ;
#11435 = CARTESIAN_POINT ( 'NONE',  ( 0.1062992125984796865, -0.1023622047244094474, -0.5909884645248143498 ) ) ;
#11436 = AXIS2_PLACEMENT_3D ( 'NONE', #4178, #1753, #3006 ) ;
#11437 = EDGE_CURVE ( 'NONE', #10323, #12947, #6555, .T. ) ;
#11438 = VERTEX_POINT ( 'NONE', #3743 ) ;
#11439 = ORIENTED_EDGE ( 'NONE', *, *, #7165, .T. ) ;
#11440 = AXIS2_PLACEMENT_3D ( 'NONE', #3807, #7188, #13451 ) ;
#11441 = EDGE_CURVE ( 'NONE', #2439, #4146, #9082, .T. ) ;
#11442 = PRODUCT_DEFINITION_CONTEXT ( 'detailed design', #5986, 'design' ) ;
#11443 = VERTEX_POINT ( 'NONE', #12343 ) ;
#11444 = VECTOR ( 'NONE', #846, 39.37007874015748143 ) ;
#11445 = DIRECTION ( 'NONE',  ( 0.000000000000000000, 1.000000000000000000, 0.000000000000000000 ) ) ;
#11446 = AXIS2_PLACEMENT_3D ( 'NONE', #976, #4646, #9437 ) ;
#11447 = DIRECTION ( 'NONE',  ( -0.000000000000000000, -1.000000000000000000, -0.000000000000000000 ) ) ;
#11448 = DIRECTION ( 'NONE',  ( -0.000000000000000000, -1.000000000000000000, -0.000000000000000000 ) ) ;
#11450 = AXIS2_PLACEMENT_3D ( 'NONE', #14400, #2484, #9776 ) ;
#11449 = CARTESIAN_POINT ( 'NONE',  ( 0.000000000000000000, 0.003937007874015860734, -0.1614173228346456879 ) ) ;
#11451 = CARTESIAN_POINT ( 'NONE',  ( 1.305118110236220152, 4.044111181948214319E-16, 0.02952755905511811330 ) ) ;
#11452 = VERTEX_POINT ( 'NONE', #13289 ) ;
#11453 = CARTESIAN_POINT ( 'NONE',  ( -1.945459748359986252, -2.745801194614591711, 0.1561691687464105693 ) ) ;
#11454 = CARTESIAN_POINT ( 'NONE',  ( -0.05905511811023625435, 2.637795275590551825, 0.03937007874015747977 ) ) ;
#11455 = CIRCLE ( 'NONE', #2196, 0.04330708661417329020 ) ;
#11456 = CARTESIAN_POINT ( 'NONE',  ( -1.387704745771440207, -0.02010536753476144939, -0.03937007874015747977 ) ) ;
#11457 = CARTESIAN_POINT ( 'NONE',  ( -1.190198933766853706, 0.3259758027579612860, 0.05905511811023622659 ) ) ;
#11458 = ORIENTED_EDGE ( 'NONE', *, *, #1125, .T. ) ;
#11459 = CYLINDRICAL_SURFACE ( 'NONE', #6165, 0.003937007874015721089 ) ;
#11460 = ORIENTED_EDGE ( 'NONE', *, *, #8442, .F. ) ;
#11461 = EDGE_CURVE ( 'NONE', #6519, #2195, #7326, .T. ) ;
#11462 = EDGE_CURVE ( 'NONE', #4326, #9812, #7075, .T. ) ;
#11463 = ORIENTED_EDGE ( 'NONE', *, *, #128, .T. ) ;
#11464 = CIRCLE ( 'NONE', #7699, 0.1614173228346456879 ) ;
#11465 = VERTEX_POINT ( 'NONE', #14402 ) ;
#11466 = CARTESIAN_POINT ( 'NONE',  ( 0.1629063847838169432, -0.4921259842519685179, 0.2122517380126066888 ) ) ;
#11467 = CARTESIAN_POINT ( 'NONE',  ( 0.000000000000000000, -0.4881889763779528324, 0.1768186671464649640 ) ) ;
#11468 = CIRCLE ( 'NONE', #9721, 0.7007874015748031260 ) ;
#11469 = EDGE_CURVE ( 'NONE', #15156, #13856, #3976, .T. ) ;
#11470 = DIRECTION ( 'NONE',  ( 0.000000000000000000, 0.000000000000000000, -1.000000000000000000 ) ) ;
#11471 = CARTESIAN_POINT ( 'NONE',  ( -0.4815353412745563833, 0.000000000000000000, 0.3552976658085854056 ) ) ;
#11472 = APPLICATION_PROTOCOL_DEFINITION ( 'draft international standard', 'automotive_design', 1998, #8597 ) ;
#11473 = CARTESIAN_POINT ( 'NONE',  ( -0.05114323250695500950, 0.000000000000000000, 0.08858267716535433989 ) ) ;
#11474 = CARTESIAN_POINT ( 'NONE',  ( 0.05114323250695503031, 0.05905511811023622659, 0.08858267716535433989 ) ) ;
#11475 = VERTEX_POINT ( 'NONE', #8674 ) ;
#11476 = LINE ( 'NONE', #10138, #13925 ) ;
#11477 = DIRECTION ( 'NONE',  ( -0.5000000000000001110, 0.000000000000000000, 0.8660254037844388186 ) ) ;
#11478 = CARTESIAN_POINT ( 'NONE',  ( -0.4769054117961255002, -0.4921259842519685179, 0.3480785096661502265 ) ) ;
#11479 = AXIS2_PLACEMENT_3D ( 'NONE', #554, #10266, #4157 ) ;
#11480 = CARTESIAN_POINT ( 'NONE',  ( -1.181102362204724310, -0.1279527559055117225, 0.02559055118110236185 ) ) ;
#11481 = AXIS2_PLACEMENT_3D ( 'NONE', #12576, #4264, #5441 ) ;
#11482 = ORIENTED_EDGE ( 'NONE', *, *, #15461, .T. ) ;
#11483 = FACE_OUTER_BOUND ( 'NONE', #6808, .T. ) ;
#11484 = EDGE_LOOP ( 'NONE', ( #3089, #2399 ) ) ;
#11485 = ORIENTED_EDGE ( 'NONE', *, *, #8077, .T. ) ;
#11486 = ADVANCED_FACE ( 'NONE', ( #13518 ), #8329, .T. ) ;
#11487 = DIRECTION ( 'NONE',  ( -0.000000000000000000, -1.000000000000000000, -0.000000000000000000 ) ) ;
#11488 = CARTESIAN_POINT ( 'NONE',  ( -1.961602614639095687, -2.845484579323528163, 0.1618271791655376268 ) ) ;
#11489 = CARTESIAN_POINT ( 'NONE',  ( -0.05114323250695500950, 0.000000000000000000, 0.08858267716535433989 ) ) ;
#11490 = CYLINDRICAL_SURFACE ( 'NONE', #5072, 0.003937007874015724558 ) ;
#11491 = LINE ( 'NONE', #821, #4652 ) ;
#11492 = LINE ( 'NONE', #2957, #6556 ) ;
#11493 = CARTESIAN_POINT ( 'NONE',  ( -2.100301733797227399, -2.106182698134460907, -0.1158666453195839885 ) ) ;
#11494 = ORIENTED_EDGE ( 'NONE', *, *, #6921, .F. ) ;
#11495 = VERTEX_POINT ( 'NONE', #9937 ) ;
#11496 = ORIENTED_EDGE ( 'NONE', *, *, #3979, .T. ) ;
#11497 = ORIENTED_EDGE ( 'NONE', *, *, #634, .T. ) ;
#11498 = CARTESIAN_POINT ( 'NONE',  ( -0.7455328141524873997, 1.190944881889763884, 0.3622425942647021779 ) ) ;
#11499 = CARTESIAN_POINT ( 'NONE',  ( 3.379785373986856012E-18, 1.043307086614173596, 1.951319995474429431E-18 ) ) ;
#11500 = EDGE_CURVE ( 'NONE', #4812, #6947, #1575, .T. ) ;
#11501 = CARTESIAN_POINT ( 'NONE',  ( 0.1181102362204724254, 2.448818897637795367, -0.03937007874015747977 ) ) ;
#11502 = DIRECTION ( 'NONE',  ( -0.000000000000000000, -1.000000000000000000, -0.000000000000000000 ) ) ;
#11503 = DIRECTION ( 'NONE',  ( 1.000000000000000000, 0.000000000000000000, 0.000000000000000000 ) ) ;
#11504 = DIRECTION ( 'NONE',  ( 0.000000000000000000, 0.000000000000000000, 1.000000000000000000 ) ) ;
#11505 = CARTESIAN_POINT ( 'NONE',  ( -1.908371742851994624, -2.849778903878224412, -0.1333857941085078158 ) ) ;
#11506 = ORIENTED_EDGE ( 'NONE', *, *, #3679, .T. ) ;
#11507 = LINE ( 'NONE', #772, #3683 ) ;
#11508 = EDGE_CURVE ( 'NONE', #13903, #10948, #3580, .T. ) ;
#11509 = CARTESIAN_POINT ( 'NONE',  ( 0.000000000000000000, 2.161417322834645827, 0.000000000000000000 ) ) ;
#11510 = DIRECTION ( 'NONE',  ( 1.000000000000000000, 0.000000000000000000, -1.224646799147353207E-16 ) ) ;
#11511 = ORIENTED_EDGE ( 'NONE', *, *, #14413, .F. ) ;
#11512 = ORIENTED_EDGE ( 'NONE', *, *, #15163, .T. ) ;
#11513 = VERTEX_POINT ( 'NONE', #6464 ) ;
#11514 = CARTESIAN_POINT ( 'NONE',  ( 0.2364476915724980366, -0.4881889763779528324, 0.06377609659104091500 ) ) ;
#11515 = EDGE_CURVE ( 'NONE', #6947, #6576, #10003, .T. ) ;
#11516 = EDGE_CURVE ( 'NONE', #12255, #13377, #14341, .T. ) ;
#11517 = LINE ( 'NONE', #2985, #5847 ) ;
#11518 = CARTESIAN_POINT ( 'NONE',  ( 0.4749369078591172966, -0.4921259842519685179, 0.3514880584999470203 ) ) ;
#11519 = DIRECTION ( 'NONE',  ( -1.000000000000000000, 0.000000000000000000, 0.000000000000000000 ) ) ;
#11520 = CARTESIAN_POINT ( 'NONE',  ( 0.2393297813660762718, -0.1023622047244094474, 0.06089400679746260342 ) ) ;
#11521 = EDGE_LOOP ( 'NONE', ( #13880, #403, #8681 ) ) ;
#11522 = DIRECTION ( 'NONE',  ( 0.000000000000000000, 0.000000000000000000, -1.000000000000000000 ) ) ;
#11523 = EDGE_CURVE ( 'NONE', #7254, #12443, #7957, .T. ) ;
#11524 = DIRECTION ( 'NONE',  ( 0.000000000000000000, 0.000000000000000000, 1.000000000000000000 ) ) ;
#11525 = DIRECTION ( 'NONE',  ( 0.000000000000000000, 1.000000000000000000, 0.000000000000000000 ) ) ;
#11526 = DIRECTION ( 'NONE',  ( -2.775557561562891351E-14, 0.5840537863392681883, 0.8117149589990099168 ) ) ;
#11527 = EDGE_LOOP ( 'NONE', ( #11581, #2213, #4423, #13002 ) ) ;
#11528 = CARTESIAN_POINT ( 'NONE',  ( -1.607606114292111199, 0.09732815221480045631, -0.07874015748031495954 ) ) ;
#11529 = VERTEX_POINT ( 'NONE', #12513 ) ;
#11530 = ORIENTED_EDGE ( 'NONE', *, *, #5675, .T. ) ;
#11531 = PRODUCT_DEFINITION_SHAPE ( 'NONE', 'NONE',  #15496 ) ;
#11532 = VERTEX_POINT ( 'NONE', #12435 ) ;
#11533 = CARTESIAN_POINT ( 'NONE',  ( -1.417802900492933782, -0.04287136159519135126, 0.1968503937007874127 ) ) ;
#11534 = CARTESIAN_POINT ( 'NONE',  ( -0.1023622047242992716, -0.09842519685039372024, -0.2482618547482104143 ) ) ;
#11535 = EDGE_CURVE ( 'NONE', #6985, #12201, #6820, .T. ) ;
#11536 = CARTESIAN_POINT ( 'NONE',  ( -0.02479723250354459035, 0.1726834024554402824, 0.005447726382808077729 ) ) ;
#11537 = DIRECTION ( 'NONE',  ( 0.000000000000000000, 1.000000000000000000, 2.212657494868377674E-16 ) ) ;
#11538 = CARTESIAN_POINT ( 'NONE',  ( 1.181102362204724310, 4.044111181948214319E-16, -0.02559055118110236185 ) ) ;
#11539 = CARTESIAN_POINT ( 'NONE',  ( -0.1022864650139100884, 0.05905511811023622659, -1.048351444896847144E-20 ) ) ;
#11540 = VERTEX_POINT ( 'NONE', #10159 ) ;
#11541 = CARTESIAN_POINT ( 'NONE',  ( -0.1618514667033796040, -0.1023622047244094474, 0.2161887458866224576 ) ) ;
#11542 = ADVANCED_FACE ( 'NONE', ( #2003 ), #10818, .F. ) ;
#11543 = ADVANCED_FACE ( 'NONE', ( #5274 ), #10087, .T. ) ;
#11544 = DIRECTION ( 'NONE',  ( 0.8011800915435203230, -0.5984233124756390687, 0.000000000000000000 ) ) ;
#11545 = LINE ( 'NONE', #11480, #8929 ) ;
#11546 = ORIENTED_EDGE ( 'NONE', *, *, #14977, .F. ) ;
#11547 = ORIENTED_EDGE ( 'NONE', *, *, #9028, .F. ) ;
#11548 = EDGE_CURVE ( 'NONE', #9404, #1672, #7327, .T. ) ;
#11549 = CARTESIAN_POINT ( 'NONE',  ( -0.5610236220472173407, -0.4921259842519685179, 0.2102555114175287954 ) ) ;
#11550 = ORIENTED_EDGE ( 'NONE', *, *, #3657, .F. ) ;
#11551 = ORIENTED_EDGE ( 'NONE', *, *, #7444, .T. ) ;
#11552 = DIRECTION ( 'NONE',  ( 0.000000000000000000, 0.000000000000000000, 1.000000000000000000 ) ) ;
#11553 = DIRECTION ( 'NONE',  ( 0.000000000000000000, 0.000000000000000000, -1.000000000000000000 ) ) ;
#11554 = B_SPLINE_CURVE_WITH_KNOTS ( 'NONE', 3,
 ( #9790, #8605, #6237, #12366 ),
 .UNSPECIFIED., .F., .F.,
 ( 4, 4 ),
 ( 0.000000000000000000, 2.119993237936687445E-05 ),
 .UNSPECIFIED. ) ;
#11555 = DIMENSIONAL_EXPONENTS ( 1.000000000000000000, 0.000000000000000000, 0.000000000000000000, 0.000000000000000000, 0.000000000000000000, 0.000000000000000000, 0.000000000000000000 ) ;
#11556 = CYLINDRICAL_SURFACE ( 'NONE', #1699, 0.03937007874015761161 ) ;
#11557 = EDGE_CURVE ( 'NONE', #10362, #12169, #3088, .T. ) ;
#11558 = CARTESIAN_POINT ( 'NONE',  ( 0.000000000000000000, 0.4133858267716535306, 0.000000000000000000 ) ) ;
#11559 = DIRECTION ( 'NONE',  ( 0.000000000000000000, 1.000000000000000000, 0.000000000000000000 ) ) ;
#11560 = CARTESIAN_POINT ( 'NONE',  ( 7.328595018519593763E-17, 1.377952755905512028, -0.5984251968503937480 ) ) ;
#11561 = CARTESIAN_POINT ( 'NONE',  ( -2.104378079979697169, -1.678226622365109222, -0.1033464566929128137 ) ) ;
#11562 = ORIENTED_EDGE ( 'NONE', *, *, #15076, .T. ) ;
#11563 = EDGE_CURVE ( 'NONE', #14453, #880, #1833, .T. ) ;
#11564 = EDGE_LOOP ( 'NONE', ( #7335, #6265 ) ) ;
#11565 = VERTEX_POINT ( 'NONE', #11314 ) ;
#11566 = ORIENTED_EDGE ( 'NONE', *, *, #14082, .F. ) ;
#11567 = B_SPLINE_CURVE_WITH_KNOTS ( 'NONE', 3,
 ( #7313, #13650, #8338, #10841 ),
 .UNSPECIFIED., .F., .F.,
 ( 4, 4 ),
 ( 0.01503324949781038346, 0.01563576546786441673 ),
 .UNSPECIFIED. ) ;
#11568 = CARTESIAN_POINT ( 'NONE',  ( -1.570493619109623262, 0.1151020441257367272, -0.05905511811023622659 ) ) ;
#11569 = DIRECTION ( 'NONE',  ( 0.000000000000000000, 0.000000000000000000, -1.000000000000000000 ) ) ;
#11570 = DIRECTION ( 'NONE',  ( -0.000000000000000000, -1.000000000000000000, -0.000000000000000000 ) ) ;
#11571 = DIRECTION ( 'NONE',  ( 1.000000000000000000, 0.000000000000000000, 0.000000000000000000 ) ) ;
#11572 = LINE ( 'NONE', #9476, #2136 ) ;
#11573 = DIRECTION ( 'NONE',  ( -1.000000000000000000, -0.000000000000000000, -0.000000000000000000 ) ) ;
#11574 = CARTESIAN_POINT ( 'NONE',  ( -1.919254730030994338, -2.820607295135873382, -0.1479486526684962999 ) ) ;
#11575 = ORIENTED_EDGE ( 'NONE', *, *, #4247, .F. ) ;
#11576 = CARTESIAN_POINT ( 'NONE',  ( 0.000000000000000000, 0.5590551181102362266, 0.000000000000000000 ) ) ;
#11577 = FACE_OUTER_BOUND ( 'NONE', #10915, .T. ) ;
#11578 = DIRECTION ( 'NONE',  ( 0.000000000000000000, -1.000000000000000000, 0.000000000000000000 ) ) ;
#11579 = ORIENTED_EDGE ( 'NONE', *, *, #8562, .F. ) ;
#11580 = ORIENTED_EDGE ( 'NONE', *, *, #14685, .T. ) ;
#11581 = ORIENTED_EDGE ( 'NONE', *, *, #10934, .F. ) ;
#11582 = CIRCLE ( 'NONE', #6064, 0.003937007874015743640 ) ;
#11583 = AXIS2_PLACEMENT_3D ( 'NONE', #1620, #6380, #66 ) ;
#11584 = DIRECTION ( 'NONE',  ( 0.000000000000000000, 0.000000000000000000, 1.000000000000000000 ) ) ;
#11585 = AXIS2_PLACEMENT_3D ( 'NONE', #15082, #4272, #5516 ) ;
#11586 = VECTOR ( 'NONE', #14301, 39.37007874015748143 ) ;
#11587 = DIRECTION ( 'NONE',  ( 0.5000000000000035527, 0.000000000000000000, -0.8660254037844365982 ) ) ;
#11588 = CARTESIAN_POINT ( 'NONE',  ( -1.947132143286702144, -2.887778429919098500, 0.1348783224627881361 ) ) ;
#11589 = CARTESIAN_POINT ( 'NONE',  ( 0.000000000000000000, 1.417322834645669438, 0.000000000000000000 ) ) ;
#11590 = DIRECTION ( 'NONE',  ( 0.000000000000000000, -0.000000000000000000, 1.000000000000000000 ) ) ;
#11591 = CARTESIAN_POINT ( 'NONE',  ( -1.496171808639726653, 0.2144740403064262224, 0.05905511811023622659 ) ) ;
#11592 = ORIENTED_EDGE ( 'NONE', *, *, #5580, .F. ) ;
#11593 = CARTESIAN_POINT ( 'NONE',  ( -0.05905511811023622659, 1.190944881889763884, -0.5946706712680680518 ) ) ;
#11594 = DIRECTION ( 'NONE',  ( 0.000000000000000000, 0.000000000000000000, 1.000000000000000000 ) ) ;
#11595 = AXIS2_PLACEMENT_3D ( 'NONE', #2635, #62, #13219 ) ;
#11596 = CIRCLE ( 'NONE', #9603, 0.04330708661417326938 ) ;
#11597 = PLANE ( 'NONE',  #8968 ) ;
#11598 = SPHERICAL_SURFACE ( 'NONE', #11333, 0.003937007874015747977 ) ;
#11599 = VERTEX_POINT ( 'NONE', #7724 ) ;
#11600 = EDGE_CURVE ( 'NONE', #3964, #15344, #15081, .T. ) ;
#11601 = AXIS2_PLACEMENT_3D ( 'NONE', #15051, #6570, #11369 ) ;
#11602 = DIRECTION ( 'NONE',  ( -0.9040582794047685722, 0.000000000000000000, 0.4274092037376938658 ) ) ;
#11603 = AXIS2_PLACEMENT_3D ( 'NONE', #1509, #6257, #871 ) ;
#11604 = EDGE_CURVE ( 'NONE', #6660, #12429, #10828, .T. ) ;
#11605 = VERTEX_POINT ( 'NONE', #1771 ) ;
#11606 = ORIENTED_EDGE ( 'NONE', *, *, #13252, .F. ) ;
#11607 = EDGE_CURVE ( 'NONE', #12818, #6858, #13687, .T. ) ;
#11608 = DIRECTION ( 'NONE',  ( 0.000000000000000000, 1.000000000000000000, 0.000000000000000000 ) ) ;
#11609 = CYLINDRICAL_SURFACE ( 'NONE', #9661, 0.03937007874015747977 ) ;
#11610 = AXIS2_PLACEMENT_3D ( 'NONE', #9005, #7809, #2700 ) ;
#11611 = AXIS2_PLACEMENT_3D ( 'NONE', #5027, #1590, #8648 ) ;
#11612 = CIRCLE ( 'NONE', #9109, 0.003937007874015741038 ) ;
#11613 = CARTESIAN_POINT ( 'NONE',  ( 0.06299212598430636856, -0.2952755905511811330, -0.4624047872104674606 ) ) ;
#11614 = DIRECTION ( 'NONE',  ( -0.9926610512904576744, -0.1209298856814283729, -0.000000000000000000 ) ) ;
#11615 = CIRCLE ( 'NONE', #13369, 0.003937007874015754916 ) ;
#11616 = DIRECTION ( 'NONE',  ( 1.000000000000000000, -1.783360582779902981E-15, 0.000000000000000000 ) ) ;
#11617 = CIRCLE ( 'NONE', #8618, 0.04527559055118110520 ) ;
#11618 = DIRECTION ( 'NONE',  ( -3.075191616504340279E-15, 0.000000000000000000, 1.000000000000000000 ) ) ;
#11619 = VERTEX_POINT ( 'NONE', #13286 ) ;
#11620 = ORIENTED_EDGE ( 'NONE', *, *, #9992, .F. ) ;
#11621 = DIRECTION ( 'NONE',  ( 0.000000000000000000, 0.000000000000000000, -1.000000000000000000 ) ) ;
#11622 = CARTESIAN_POINT ( 'NONE',  ( -0.2652685895081163259, -0.1023622047244094474, 0.03495519865516327068 ) ) ;
#11623 = EDGE_CURVE ( 'NONE', #3451, #10948, #14946, .T. ) ;
#11624 = DIRECTION ( 'NONE',  ( 0.000000000000000000, 1.000000000000000000, 0.000000000000000000 ) ) ;
#11625 = ORIENTED_EDGE ( 'NONE', *, *, #12766, .T. ) ;
#11626 = VECTOR ( 'NONE', #806, 39.37007874015748143 ) ;
#11627 = VECTOR ( 'NONE', #9208, 39.37007874015748143 ) ;
#11628 = CIRCLE ( 'NONE', #5099, 0.003937007874015724558 ) ;
#11629 = ADVANCED_FACE ( 'NONE', ( #1930 ), #11490, .T. ) ;
#11630 = VECTOR ( 'NONE', #15203, 39.37007874015748143 ) ;
#11631 = EDGE_LOOP ( 'NONE', ( #11375, #4921, #9400, #4959 ) ) ;
#11632 = AXIS2_PLACEMENT_3D ( 'NONE', #9086, #13865, #15115 ) ;
#11633 = CYLINDRICAL_SURFACE ( 'NONE', #1064, 0.03937007874015751446 ) ;
#11634 = VERTEX_POINT ( 'NONE', #4037 ) ;
#11635 = CIRCLE ( 'NONE', #8130, 0.1614173228346456879 ) ;
#11636 = ORIENTED_EDGE ( 'NONE', *, *, #8843, .T. ) ;
#11637 = EDGE_CURVE ( 'NONE', #3832, #4717, #14598, .T. ) ;
#11638 = VERTEX_POINT ( 'NONE', #9056 ) ;
#11639 = CARTESIAN_POINT ( 'NONE',  ( 0.000000000000000000, 0.07874015748031495954, 0.000000000000000000 ) ) ;
#11640 = DIRECTION ( 'NONE',  ( -0.000000000000000000, -1.000000000000000000, -0.000000000000000000 ) ) ;
#11641 = AXIS2_PLACEMENT_3D ( 'NONE', #7687, #14673, #1737 ) ;
#11642 = AXIS2_PLACEMENT_3D ( 'NONE', #14519, #7233, #14284 ) ;
#11643 = DIRECTION ( 'NONE',  ( -8.673617379884029309E-17, -1.000000000000000000, 0.000000000000000000 ) ) ;
#11644 = VECTOR ( 'NONE', #3036, 39.37007874015748143 ) ;
#11645 = CARTESIAN_POINT ( 'NONE',  ( -1.190198933766853706, 0.3259758027579612860, 0.05905511811023622659 ) ) ;
#11646 = CARTESIAN_POINT ( 'NONE',  ( 1.181102362204724310, 0.1240157480314963978, -0.02559055118110236185 ) ) ;
#11647 = AXIS2_PLACEMENT_3D ( 'NONE', #15333, #4453, #4521 ) ;
#11648 = CARTESIAN_POINT ( 'NONE',  ( -0.07874015748031543138, -0.1682792322177920907, 0.05905511811023622659 ) ) ;
#11649 = VERTEX_POINT ( 'NONE', #3186 ) ;
#11650 = ORIENTED_EDGE ( 'NONE', *, *, #6147, .T. ) ;
#11651 = CIRCLE ( 'NONE', #12160, 0.5826771653543306728 ) ;
#11652 = ORIENTED_EDGE ( 'NONE', *, *, #5861, .F. ) ;
#11653 = CIRCLE ( 'NONE', #9900, 0.003937007874015750579 ) ;
#11654 = CIRCLE ( 'NONE', #13654, 0.007874015748031501158 ) ;
#11655 = EDGE_LOOP ( 'NONE', ( #13297, #8755, #11946, #2277 ) ) ;
#11656 = EDGE_CURVE ( 'NONE', #9755, #2740, #10595, .T. ) ;
#11657 = AXIS2_PLACEMENT_3D ( 'NONE', #6062, #3742, #14628 ) ;
#11658 = CARTESIAN_POINT ( 'NONE',  ( 0.000000000000000000, -0.1023622047244094474, 0.000000000000000000 ) ) ;
#11659 = DIRECTION ( 'NONE',  ( 0.000000000000000000, 0.000000000000000000, -1.000000000000000000 ) ) ;
#11660 = FACE_OUTER_BOUND ( 'NONE', #10322, .T. ) ;
#11661 = DIRECTION ( 'NONE',  ( 0.5000000000000002220, 0.000000000000000000, -0.8660254037844384856 ) ) ;
#11662 = EDGE_CURVE ( 'NONE', #1599, #10400, #9094, .T. ) ;
#11663 = FACE_OUTER_BOUND ( 'NONE', #7965, .T. ) ;
#11664 = AXIS2_PLACEMENT_3D ( 'NONE', #8514, #6155, #5045 ) ;
#11665 = DIRECTION ( 'NONE',  ( 0.4999999999999975575, 0.000000000000000000, 0.8660254037844399289 ) ) ;
#11666 = CIRCLE ( 'NONE', #5397, 2.814960629921260171 ) ;
#11667 = CARTESIAN_POINT ( 'NONE',  ( -1.916688711786504351, -2.827624850986260263, -0.1689233196601243048 ) ) ;
#11668 = AXIS2_PLACEMENT_3D ( 'NONE', #4189, #6369, #14840 ) ;
#11669 = VERTEX_POINT ( 'NONE', #1843 ) ;
#11670 = CARTESIAN_POINT ( 'NONE',  ( 0.1724006475077543565, -0.1023622047244094474, 0.1768186671464649640 ) ) ;
#11671 = LINE ( 'NONE', #10491, #1400 ) ;
#11672 = DIMENSIONAL_EXPONENTS ( 1.000000000000000000, 0.000000000000000000, 0.000000000000000000, 0.000000000000000000, 0.000000000000000000, 0.000000000000000000, 0.000000000000000000 ) ;
#11673 = CIRCLE ( 'NONE', #14683, 0.003937007874015741038 ) ;
#11674 = PRODUCT_DEFINITION_SHAPE ( 'NONE', 'NONE',  #15471 ) ;
#11675 = ORIENTED_EDGE ( 'NONE', *, *, #271, .F. ) ;
#11676 = EDGE_LOOP ( 'NONE', ( #12091, #14282 ) ) ;
#11677 = EDGE_LOOP ( 'NONE', ( #2396, #15070, #5826, #9030, #3749 ) ) ;
#11678 = AXIS2_PLACEMENT_3D ( 'NONE', #9444, #810, #8186 ) ;
#11679 = DIRECTION ( 'NONE',  ( 0.000000000000000000, 0.000000000000000000, 1.000000000000000000 ) ) ;
#11680 = CIRCLE ( 'NONE', #4425, 0.003937007874015724558 ) ;
#11681 = CARTESIAN_POINT ( 'NONE',  ( -0.4591888763630547210, -0.4921259842519685179, 0.3787644491703232585 ) ) ;
#11682 = ADVANCED_FACE ( 'NONE', ( #13584 ), #6287, .T. ) ;
#11683 = CARTESIAN_POINT ( 'NONE',  ( -1.956909830981848453, -2.859374696368682578, -0.1547382899828209646 ) ) ;
#11684 = CIRCLE ( 'NONE', #4922, 0.01968503937007875723 ) ;
#11685 = DIRECTION ( 'NONE',  ( 0.000000000000000000, 0.000000000000000000, 1.000000000000000000 ) ) ;
#11686 = CARTESIAN_POINT ( 'NONE',  ( -0.05905511811023622659, 1.338582677165354395, -0.8267716535433070613 ) ) ;
#11687 = ORIENTED_EDGE ( 'NONE', *, *, #13553, .T. ) ;
#11688 = DIRECTION ( 'NONE',  ( 0.8660254037844399289, 0.000000000000000000, 0.4999999999999975575 ) ) ;
#11689 = CARTESIAN_POINT ( 'NONE',  ( -0.06604848736013260724, 1.346456692913385877, -0.5868460571724354313 ) ) ;
#11690 = TOROIDAL_SURFACE ( 'NONE', #2423, 0.04330708661417328326, 0.003937007874015747977 ) ;
#11691 = DIRECTION ( 'NONE',  ( -0.000000000000000000, -1.000000000000000000, -0.000000000000000000 ) ) ;
#11692 = FACE_OUTER_BOUND ( 'NONE', #2110, .T. ) ;
#11693 = ORIENTED_EDGE ( 'NONE', *, *, #5556, .T. ) ;
#11694 = CARTESIAN_POINT ( 'NONE',  ( 0.9851651268172137987, -1.725292181286280480, 0.1033464566929129524 ) ) ;
#11695 = AXIS2_PLACEMENT_3D ( 'NONE', #12297, #14804, #1647 ) ;
#11696 = ORIENTED_EDGE ( 'NONE', *, *, #7023, .T. ) ;
#11697 = AXIS2_PLACEMENT_3D ( 'NONE', #3241, #2933, #3162 ) ;
#11698 = VERTEX_POINT ( 'NONE', #7723 ) ;
#11699 = EDGE_LOOP ( 'NONE', ( #13694, #3967, #2433, #15253 ) ) ;
#11700 = DIRECTION ( 'NONE',  ( 0.4999999999999975575, 0.000000000000000000, 0.8660254037844399289 ) ) ;
#11701 = CARTESIAN_POINT ( 'NONE',  ( 0.4749369078591172411, -0.09842519685039370636, 0.3514880584999470203 ) ) ;
#11702 = AXIS2_PLACEMENT_3D ( 'NONE', #6740, #4632, #3466 ) ;
#11703 = EDGE_CURVE ( 'NONE', #4548, #715, #12096, .T. ) ;
#11704 = CARTESIAN_POINT ( 'NONE',  ( -0.01753362615437414548, 0.1513390073936909108, -0.03062283071528134476 ) ) ;
#11705 = CYLINDRICAL_SURFACE ( 'NONE', #4611, 0.5905511811023621549 ) ;
#11706 = ITEM_DEFINED_TRANSFORMATION ( 'NONE', 'NONE', #3365,  #11481 ) ;
#11707 = CARTESIAN_POINT ( 'NONE',  ( -1.591501945092674841, 0.08600752902535303834, 0.1968503937007874127 ) ) ;
#11708 = AXIS2_PLACEMENT_3D ( 'NONE', #3247, #2057, #7373 ) ;
#11709 = EDGE_CURVE ( 'NONE', #8494, #6177, #370, .T. ) ;
#11710 = DIRECTION ( 'NONE',  ( 0.000000000000000000, 0.000000000000000000, -1.000000000000000000 ) ) ;
#11711 = EDGE_LOOP ( 'NONE', ( #204, #6280, #8014, #15327 ) ) ;
#11712 = CARTESIAN_POINT ( 'NONE',  ( -1.965820533970300543, -2.881262407559504801, -0.1403303144071717523 ) ) ;
#11713 = FACE_OUTER_BOUND ( 'NONE', #9307, .T. ) ;
#11714 = DIRECTION ( 'NONE',  ( 3.942553354492736135E-16, 0.000000000000000000, -1.000000000000000000 ) ) ;
#11715 = DIRECTION ( 'NONE',  ( 0.000000000000000000, -1.000000000000000000, 0.000000000000000000 ) ) ;
#11716 = EDGE_CURVE ( 'NONE', #8918, #5548, #11596, .T. ) ;
#11717 = FILL_AREA_STYLE ('',( #982 ) ) ;
#11718 = EDGE_LOOP ( 'NONE', ( #9015, #8317, #11891 ) ) ;
#11719 = AXIS2_PLACEMENT_3D ( 'NONE', #14944, #7874, #14850 ) ;
#11720 = ORIENTED_EDGE ( 'NONE', *, *, #10820, .F. ) ;
#11721 = CARTESIAN_POINT ( 'NONE',  ( -0.04921259842519618705, -0.4921259842519685179, 0.08523872084492388479 ) ) ;
#11722 = ORIENTED_EDGE ( 'NONE', *, *, #3722, .F. ) ;
#11723 = AXIS2_PLACEMENT_3D ( 'NONE', #2504, #6090, #3610 ) ;
#11724 = ORIENTED_EDGE ( 'NONE', *, *, #7416, .T. ) ;
#11725 = ORIENTED_EDGE ( 'NONE', *, *, #10759, .F. ) ;
#11726 = DIRECTION ( 'NONE',  ( -0.000000000000000000, 1.000000000000000000, 0.000000000000000000 ) ) ;
#11727 = CARTESIAN_POINT ( 'NONE',  ( 0.1618514667033794374, -0.4921259842519685179, 0.2083147301385909200 ) ) ;
#11728 = DIRECTION ( 'NONE',  ( -0.000000000000000000, -0.000000000000000000, -1.000000000000000000 ) ) ;
#11729 = EDGE_CURVE ( 'NONE', #14746, #9379, #8839, .T. ) ;
#11730 = DIRECTION ( 'NONE',  ( 0.000000000000000000, 0.000000000000000000, 1.000000000000000000 ) ) ;
#11731 = CARTESIAN_POINT ( 'NONE',  ( -0.05905511811012607165, -0.09842519685039370636, -2.134256245046224357E-17 ) ) ;
#11732 = AXIS2_PLACEMENT_3D ( 'NONE', #12545, #864, #11590 ) ;
#11733 = ADVANCED_FACE ( 'NONE', ( #594, #14782, #14945 ), #8748, .F. ) ;
#11734 = DIRECTION ( 'NONE',  ( 0.000000000000000000, 0.000000000000000000, -1.000000000000000000 ) ) ;
#11735 = CYLINDRICAL_SURFACE ( 'NONE', #4147, 0.003937007874015741038 ) ;
#11736 = CARTESIAN_POINT ( 'NONE',  ( 1.181102362204724310, 4.044111181948214319E-16, 0.02952755905511811330 ) ) ;
#11737 = CARTESIAN_POINT ( 'NONE',  ( -0.05905511811023622659, 1.043307086614173373, -0.5511811023622047445 ) ) ;
#11738 = CIRCLE ( 'NONE', #5960, 0.003937007874015758385 ) ;
#11739 = ADVANCED_FACE ( 'NONE', ( #461 ), #7380, .T. ) ;
#11740 = CYLINDRICAL_SURFACE ( 'NONE', #3836, 0.003937007874015724558 ) ;
#11741 = DIRECTION ( 'NONE',  ( -1.060575238724906792E-16, 1.000000000000000000, 6.123233995736767268E-17 ) ) ;
#11742 = EDGE_LOOP ( 'NONE', ( #14434, #2381, #2309, #13601 ) ) ;
#11743 = ORIENTED_EDGE ( 'NONE', *, *, #7014, .T. ) ;
#11744 = ORIENTED_EDGE ( 'NONE', *, *, #6946, .T. ) ;
#11745 = EDGE_LOOP ( 'NONE', ( #5878, #7542, #15131, #7252 ) ) ;
#11746 = CARTESIAN_POINT ( 'NONE',  ( -1.568343923620152180, 0.1178486908565802016, -0.05905511811023622659 ) ) ;
#11747 = CARTESIAN_POINT ( 'NONE',  ( -1.276200637803905691, -0.1988000726501942539, 0.03937007874015747977 ) ) ;
#11748 = EDGE_CURVE ( 'NONE', #10074, #12909, #10380, .T. ) ;
#11749 = CARTESIAN_POINT ( 'NONE',  ( -0.06144837730694100580, 0.1461156186057984141, 0.05762996311186435044 ) ) ;
#11750 = CARTESIAN_POINT ( 'NONE',  ( -0.5405798186813893791, 1.344775570699144218, 0.2377539613194186996 ) ) ;
#11751 = CYLINDRICAL_SURFACE ( 'NONE', #3819, 0.003937007874015743640 ) ;
#11752 = DIRECTION ( 'NONE',  ( 0.000000000000000000, 0.000000000000000000, 1.000000000000000000 ) ) ;
#11753 = ORIENTED_EDGE ( 'NONE', *, *, #4650, .T. ) ;
#11754 = DIRECTION ( 'NONE',  ( -1.000000000000000000, -0.000000000000000000, -3.476578583725179813E-16 ) ) ;
#11755 = EDGE_CURVE ( 'NONE', #4395, #10762, #10898, .T. ) ;
#11756 = CARTESIAN_POINT ( 'NONE',  ( -0.06692913385815731087, -0.2952755905511811330, -0.3757906139821208247 ) ) ;
#11757 = CARTESIAN_POINT ( 'NONE',  ( 1.220472440944881720, 4.092325622859527280E-16, 0.02952755905511811330 ) ) ;
#11758 = VERTEX_POINT ( 'NONE', #13683 ) ;
#11759 = ORIENTED_EDGE ( 'NONE', *, *, #1698, .T. ) ;
#11760 = ADVANCED_FACE ( 'NONE', ( #9135 ), #2001, .T. ) ;
#11761 = EDGE_LOOP ( 'NONE', ( #1583, #12178 ) ) ;
#11762 = DIRECTION ( 'NONE',  ( 1.060575238724906792E-16, 1.000000000000000000, -6.123233995736764803E-17 ) ) ;
#11763 = DIRECTION ( 'NONE',  ( 0.000000000000000000, 0.000000000000000000, -1.000000000000000000 ) ) ;
#11764 = DIRECTION ( 'NONE',  ( 0.8144815189573203495, -0.5801894994542524664, 1.283760644411384150E-16 ) ) ;
#11765 = CARTESIAN_POINT ( 'NONE',  ( -0.4751993499419962519, 1.346456692913385877, 0.3506226965216301950 ) ) ;
#11766 = B_SPLINE_CURVE_WITH_KNOTS ( 'NONE', 3,
 ( #1109, #1976, #14030, #9325 ),
 .UNSPECIFIED., .F., .F.,
 ( 4, 4 ),
 ( 0.0001112824830758690162, 0.0003582764151311783850 ),
 .UNSPECIFIED. ) ;
#11767 = CARTESIAN_POINT ( 'NONE',  ( -1.185456167499539193, 0.3350708678521160944, -0.05695194461256634227 ) ) ;
#11768 = VERTEX_POINT ( 'NONE', #2950 ) ;
#11769 = DIRECTION ( 'NONE',  ( 4.292327424963298981E-16, -1.000000000000000000, -2.478176394252600369E-16 ) ) ;
#11770 = CARTESIAN_POINT ( 'NONE',  ( 0.1023622047244639455, -0.1023622047244094474, -0.5870514566507987197 ) ) ;
#11771 = CARTESIAN_POINT ( 'NONE',  ( -1.607347250558628149, 0.09769655912556320099, 0.07190431746647057976 ) ) ;
#11772 = ORIENTED_EDGE ( 'NONE', *, *, #5756, .F. ) ;
#11773 = DIRECTION ( 'NONE',  ( 0.000000000000000000, 1.000000000000000000, 2.222614453595283597E-16 ) ) ;
#11774 = ORIENTED_EDGE ( 'NONE', *, *, #3386, .T. ) ;
#11775 = ADVANCED_FACE ( 'NONE', ( #6603 ), #10338, .F. ) ;
#11776 = ORIENTED_EDGE ( 'NONE', *, *, #1117, .F. ) ;
#11777 = VERTEX_POINT ( 'NONE', #7954 ) ;
#11778 = ORIENTED_EDGE ( 'NONE', *, *, #4244, .T. ) ;
#11779 = CARTESIAN_POINT ( 'NONE',  ( 0.000000000000000000, 1.417322834645669438, 0.000000000000000000 ) ) ;
#11780 = DIRECTION ( 'NONE',  ( 1.000000000000000000, 0.000000000000000000, 0.000000000000000000 ) ) ;
#11781 = CARTESIAN_POINT ( 'NONE',  ( 0.1638199706403873079, -0.4881889763779528324, 0.2127791970528254417 ) ) ;
#11782 = DIRECTION ( 'NONE',  ( 1.000000000000000000, 0.000000000000000000, 1.445602896647339903E-16 ) ) ;
#11783 = CONTEXT_DEPENDENT_SHAPE_REPRESENTATION ( #6693, #9287 ) ;
#11784 = CARTESIAN_POINT ( 'NONE',  ( -0.05905511811012598145, -0.09842519685039370636, -0.2377126739438355507 ) ) ;
#11785 = CARTESIAN_POINT ( 'NONE',  ( -0.03213667549430108267, -0.1820030000337380105, 0.02170016096604327621 ) ) ;
#11786 = ORIENTED_EDGE ( 'NONE', *, *, #2044, .T. ) ;
#11787 = DIRECTION ( 'NONE',  ( -0.8483823383050520528, -0.5293839892290402860, -0.000000000000000000 ) ) ;
#11788 = CARTESIAN_POINT ( 'NONE',  ( -1.293236445124221312, 0.1355266887446167634, -0.05905511811023622659 ) ) ;
#11789 = DIRECTION ( 'NONE',  ( 0.000000000000000000, 0.000000000000000000, 1.000000000000000000 ) ) ;
#11790 = ORIENTED_EDGE ( 'NONE', *, *, #1481, .F. ) ;
#11791 = LINE ( 'NONE', #15310, #12692 ) ;
#11792 = ORIENTED_EDGE ( 'NONE', *, *, #3883, .F. ) ;
#11793 = VERTEX_POINT ( 'NONE', #817 ) ;
#11794 = ORIENTED_EDGE ( 'NONE', *, *, #8166, .T. ) ;
#11795 = DIRECTION ( 'NONE',  ( 1.971276677246368068E-16, 0.000000000000000000, -1.000000000000000000 ) ) ;
#11796 = EDGE_CURVE ( 'NONE', #7594, #25, #343, .T. ) ;
#11797 = CARTESIAN_POINT ( 'NONE',  ( 0.000000000000000000, 0.000000000000000000, 0.000000000000000000 ) ) ;
#11798 = CARTESIAN_POINT ( 'NONE',  ( 7.183951695785653893E-17, -1.707404996040164512E-17, -0.5826771653543306728 ) ) ;
#11799 = DIRECTION ( 'NONE',  ( 1.000000000000000000, 0.000000000000000000, 0.000000000000000000 ) ) ;
#11800 = DIRECTION ( 'NONE',  ( -0.4999999999999798495, 0.000000000000000000, 0.8660254037844502539 ) ) ;
#11801 = DIRECTION ( 'NONE',  ( -0.000000000000000000, -0.000000000000000000, -1.000000000000000000 ) ) ;
#11802 = CARTESIAN_POINT ( 'NONE',  ( 0.2373612774290684013, -0.4881889763779528324, 0.06430355563125962626 ) ) ;
#11803 = FACE_OUTER_BOUND ( 'NONE', #10420, .T. ) ;
#11804 = DIRECTION ( 'NONE',  ( -0.000000000000000000, 0.000000000000000000, 1.000000000000000000 ) ) ;
#11805 = ORIENTED_EDGE ( 'NONE', *, *, #15091, .T. ) ;
#11806 = EDGE_CURVE ( 'NONE', #3700, #9513, #2068, .T. ) ;
#11807 = ORIENTED_EDGE ( 'NONE', *, *, #5096, .F. ) ;
#11808 = ORIENTED_EDGE ( 'NONE', *, *, #3019, .F. ) ;
#11809 = ADVANCED_FACE ( 'NONE', ( #910 ), #14295, .F. ) ;
#11810 = ORIENTED_EDGE ( 'NONE', *, *, #13998, .F. ) ;
#11811 =( REPRESENTATION_RELATIONSHIP ('NONE','NONE', #8904, #7785 ) REPRESENTATION_RELATIONSHIP_WITH_TRANSFORMATION ( #12869 )SHAPE_REPRESENTATION_RELATIONSHIP( ) );
#11812 = EDGE_CURVE ( 'NONE', #2760, #677, #9591, .T. ) ;
#11813 = DIRECTION ( 'NONE',  ( 1.000000000000000000, 0.000000000000000000, 3.973232667114495301E-16 ) ) ;
#11814 = CYLINDRICAL_SURFACE ( 'NONE', #446, 0.003937007874015758385 ) ;
#11815 = CARTESIAN_POINT ( 'NONE',  ( 0.4788739157331329821, -0.09448818897637796532, 0.3446689608323530440 ) ) ;
#11816 = DIRECTION ( 'NONE',  ( 0.8660254037844390407, 0.000000000000000000, -0.4999999999999995004 ) ) ;
#11817 = DIRECTION ( 'NONE',  ( 0.000000000000000000, 0.000000000000000000, 1.000000000000000000 ) ) ;
#11818 = ORIENTED_EDGE ( 'NONE', *, *, #14391, .F. ) ;
#11819 = DIRECTION ( 'NONE',  ( 0.000000000000000000, 1.000000000000000000, 0.000000000000000000 ) ) ;
#11820 = CARTESIAN_POINT ( 'NONE',  ( -0.4606299212598437554, -0.4881889763779528324, 0.3841425019411281450 ) ) ;
#11821 = CIRCLE ( 'NONE', #9064, 0.03937007874015747977 ) ;
#11822 = EDGE_LOOP ( 'NONE', ( #8416, #12609, #4171, #15309 ) ) ;
#11823 = EDGE_CURVE ( 'NONE', #8019, #10712, #13151, .T. ) ;
#11824 = ORIENTED_EDGE ( 'NONE', *, *, #13960, .F. ) ;
#11825 = EDGE_CURVE ( 'NONE', #4883, #10896, #4836, .T. ) ;
#11826 = ORIENTED_EDGE ( 'NONE', *, *, #2311, .T. ) ;
#11827 = CARTESIAN_POINT ( 'NONE',  ( 0.000000000000000000, 0.3464566929133857109, 0.000000000000000000 ) ) ;
#11828 = EDGE_CURVE ( 'NONE', #13463, #8212, #4585, .T. ) ;
#11829 = CARTESIAN_POINT ( 'NONE',  ( 0.1023622047244638761, -0.2952755905511811330, -0.3757906139821208247 ) ) ;
#11830 = CARTESIAN_POINT ( 'NONE',  ( -0.05175539059627463218, 0.06736074103232447818, 0.07475334604056275978 ) ) ;
#11831 = CARTESIAN_POINT ( 'NONE',  ( -0.1023622047242992716, -0.4881889763779528324, -0.2472069366677729363 ) ) ;
#11832 = CARTESIAN_POINT ( 'NONE',  ( -2.077823265817535514, -2.289991437693742249, 0.1278967700780702654 ) ) ;
#11833 = ORIENTED_EDGE ( 'NONE', *, *, #4244, .F. ) ;
#11834 = CARTESIAN_POINT ( 'NONE',  ( 0.5424653753748086560, 1.043012296488531332, 0.2450015538227508782 ) ) ;
#11835 = DIRECTION ( 'NONE',  ( 0.8660254037844362651, 0.000000000000000000, -0.5000000000000038858 ) ) ;
#11836 = FACE_OUTER_BOUND ( 'NONE', #6006, .T. ) ;
#11837 = CARTESIAN_POINT ( 'NONE',  ( -1.607606114292110977, 0.09732815221480028978, 0.07528365722483934541 ) ) ;
#11838 = VERTEX_POINT ( 'NONE', #9527 ) ;
#11839 = AXIS2_PLACEMENT_3D ( 'NONE', #13142, #2410, #1171 ) ;
#11840 = ORIENTED_EDGE ( 'NONE', *, *, #12383, .T. ) ;
#11841 = VECTOR ( 'NONE', #3898, 39.37007874015748143 ) ;
#11842 = EDGE_LOOP ( 'NONE', ( #13675, #2129, #15435, #9893 ) ) ;
#11843 = VECTOR ( 'NONE', #6939, 39.37007874015748143 ) ;
#11844 = ORIENTED_EDGE ( 'NONE', *, *, #8508, .T. ) ;
#11845 = ORIENTED_EDGE ( 'NONE', *, *, #1773, .T. ) ;
#11846 = ADVANCED_FACE ( 'NONE', ( #15245 ), #14146, .T. ) ;
#11847 = DIRECTION ( 'NONE',  ( 0.000000000000000000, 1.000000000000000000, -0.000000000000000000 ) ) ;
#11848 = CARTESIAN_POINT ( 'NONE',  ( -0.09842519685028335019, -0.2952755905511811330, -0.4190977005962941981 ) ) ;
#11849 = DIRECTION ( 'NONE',  ( 0.8660254037844385966, 0.000000000000000000, 0.5000000000000000000 ) ) ;
#11850 = DIRECTION ( 'NONE',  ( 1.000000000000000000, 0.000000000000000000, 0.000000000000000000 ) ) ;
#11851 = ITEM_DEFINED_TRANSFORMATION ( 'NONE', 'NONE', #7357,  #11481 ) ;
#11852 = CARTESIAN_POINT ( 'NONE',  ( 6.489392865857486264E-18, 0.07874015748031495954, 0.05298991407461853265 ) ) ;
#11853 = AXIS2_PLACEMENT_3D ( 'NONE', #11658, #12755, #2010 ) ;
#11854 = VECTOR ( 'NONE', #595, 39.37007874015748143 ) ;
#11855 = CARTESIAN_POINT ( 'NONE',  ( 1.305118110236220152, 4.044111181948214319E-16, -0.02559055118110236185 ) ) ;
#11856 = EDGE_CURVE ( 'NONE', #14202, #15217, #13340, .T. ) ;
#11857 = VERTEX_POINT ( 'NONE', #11798 ) ;
#11858 = CARTESIAN_POINT ( 'NONE',  ( 0.1259842519685039353, 2.448818897637795367, 0.03937007874015747977 ) ) ;
#11859 = AXIS2_PLACEMENT_3D ( 'NONE', #4165, #8961, #4238 ) ;
#11860 = EDGE_CURVE ( 'NONE', #9228, #675, #3332, .T. ) ;
#11861 = TOROIDAL_SURFACE ( 'NONE', #5581, 0.007874015748031495954, 0.003937007874015747977 ) ;
#11862 = DIRECTION ( 'NONE',  ( -1.000000000000000000, 0.000000000000000000, 0.000000000000000000 ) ) ;
#11863 = LENGTH_MEASURE_WITH_UNIT ( LENGTH_MEASURE( 0.02539999999999999897 ), #12960 );
#11864 = CARTESIAN_POINT ( 'NONE',  ( -0.07874015748031543138, -0.1682792322177920907, 0.03937007874015747977 ) ) ;
#11865 = ORIENTED_EDGE ( 'NONE', *, *, #13815, .T. ) ;
#11866 = CARTESIAN_POINT ( 'NONE',  ( 0.5905511811023622659, -0.2952755905511811330, -0.4190977005962939206 ) ) ;
#11868 = ORIENTED_EDGE ( 'NONE', *, *, #5360, .F. ) ;
#11867 = AXIS2_PLACEMENT_3D ( 'NONE', #5523, #8216, #5828 ) ;
#11869 = VECTOR ( 'NONE', #14229, 39.37007874015748143 ) ;
#11870 = ORIENTED_EDGE ( 'NONE', *, *, #1188, .F. ) ;
#11871 = TOROIDAL_SURFACE ( 'NONE', #7847, 0.007874015748031495954, 0.003937007874015747977 ) ;
#11872 = VERTEX_POINT ( 'NONE', #11964 ) ;
#11873 = AXIS2_PLACEMENT_3D ( 'NONE', #9418, #3461, #1106 ) ;
#11874 = FACE_OUTER_BOUND ( 'NONE', #7021, .T. ) ;
#11875 = DIRECTION ( 'NONE',  ( 1.000000000000000000, 0.000000000000000000, 0.000000000000000000 ) ) ;
#11876 = CARTESIAN_POINT ( 'NONE',  ( -1.919773973138744205, -2.887845448549585470, -0.1348206780894404822 ) ) ;
#11877 = DIMENSIONAL_EXPONENTS ( 1.000000000000000000, 0.000000000000000000, 0.000000000000000000, 0.000000000000000000, 0.000000000000000000, 0.000000000000000000, 0.000000000000000000 ) ;
#11878 = LINE ( 'NONE', #6045, #1113 ) ;
#11879 = CYLINDRICAL_SURFACE ( 'NONE', #1167, 0.003937007874015724558 ) ;
#11880 = PRODUCT_RELATED_PRODUCT_CATEGORY ( 'part', '', ( #1908 ) ) ;
#11881 = DIRECTION ( 'NONE',  ( -1.000000000000000000, 0.000000000000000000, 0.000000000000000000 ) ) ;
#11882 = AXIS2_PLACEMENT_3D ( 'NONE', #13777, #3204, #840 ) ;
#11883 = AXIS2_PLACEMENT_3D ( 'NONE', #6050, #2619, #10839 ) ;
#11884 = AXIS2_PLACEMENT_3D ( 'NONE', #721, #6888, #4230 ) ;
#11885 = DIRECTION ( 'NONE',  ( -0.000000000000000000, 0.000000000000000000, 1.000000000000000000 ) ) ;
#11886 = CARTESIAN_POINT ( 'NONE',  ( 0.000000000000000000, 0.000000000000000000, 0.000000000000000000 ) ) ;
#11887 = CIRCLE ( 'NONE', #5105, 0.007874015748031449116 ) ;
#11888 = EDGE_LOOP ( 'NONE', ( #1561, #938, #6960, #9883 ) ) ;
#11889 = ORIENTED_EDGE ( 'NONE', *, *, #8552, .F. ) ;
#11890 = ORIENTED_EDGE ( 'NONE', *, *, #7232, .T. ) ;
#11891 = ORIENTED_EDGE ( 'NONE', *, *, #12409, .T. ) ;
#11892 = ORIENTED_EDGE ( 'NONE', *, *, #8854, .T. ) ;
#11893 = AXIS2_PLACEMENT_3D ( 'NONE', #14532, #4520, #9302 ) ;
#11894 = CIRCLE ( 'NONE', #4372, 0.003937007874015750579 ) ;
#11895 = AXIS2_PLACEMENT_3D ( 'NONE', #3838, #15457, #2671 ) ;
#11896 = LINE ( 'NONE', #3666, #10352 ) ;
#11897 = AXIS2_PLACEMENT_3D ( 'NONE', #3527, #8297, #9174 ) ;
#11898 = CYLINDRICAL_SURFACE ( 'NONE', #7686, 3.169291338582677753 ) ;
#11899 = ADVANCED_FACE ( 'NONE', ( #1226 ), #3867, .T. ) ;
#11900 = DIRECTION ( 'NONE',  ( 0.7632379718484426645, 0.6461174802841010978, 0.000000000000000000 ) ) ;
#11901 = SPHERICAL_SURFACE ( 'NONE', #7565, 0.01968503937007873988 ) ;
#11902 = CARTESIAN_POINT ( 'NONE',  ( 0.000000000000000000, 0.3070866141732283561, 0.000000000000000000 ) ) ;
#11903 = EDGE_CURVE ( 'NONE', #15013, #12057, #6568, .T. ) ;
#11904 = EDGE_LOOP ( 'NONE', ( #1711, #4374, #9580, #11652 ) ) ;
#11905 =( LENGTH_UNIT ( ) NAMED_UNIT ( * ) SI_UNIT ( $, .METRE. ) );
#11906 = DIRECTION ( 'NONE',  ( -0.8660254037844405950, 3.174764303743843882E-15, 0.4999999999999967804 ) ) ;
#11907 = DIRECTION ( 'NONE',  ( 0.4999999999999979461, 0.000000000000000000, 0.8660254037844398178 ) ) ;
#11908 = CIRCLE ( 'NONE', #13149, 0.003937007874015741038 ) ;
#11909 = AXIS2_PLACEMENT_3D ( 'NONE', #4458, #1573, #5170 ) ;
#11910 = AXIS2_PLACEMENT_3D ( 'NONE', #5104, #7467, #12259 ) ;
#11911 = VERTEX_POINT ( 'NONE', #11146 ) ;
#11912 = EDGE_CURVE ( 'NONE', #9358, #6772, #103, .T. ) ;
#11913 = ORIENTED_EDGE ( 'NONE', *, *, #2199, .T. ) ;
#11914 = AXIS2_PLACEMENT_3D ( 'NONE', #12367, #4217, #8835 ) ;
#11915 = ORIENTED_EDGE ( 'NONE', *, *, #4, .T. ) ;
#11916 = DIRECTION ( 'NONE',  ( 0.5984233124757279976, 0.8011800915434538206, 0.000000000000000000 ) ) ;
#11917 = CIRCLE ( 'NONE', #12659, 0.1181102362204724532 ) ;
#11918 = CARTESIAN_POINT ( 'NONE',  ( -1.926054244504965984, -2.946671621383704309, 0.03215668881446384630 ) ) ;
#11919 = AXIS2_PLACEMENT_3D ( 'NONE', #14487, #6158, #3981 ) ;
#11920 = VECTOR ( 'NONE', #9585, 39.37007874015748143 ) ;
#11921 = ADVANCED_FACE ( 'NONE', ( #1452 ), #12835, .T. ) ;
#11922 = CARTESIAN_POINT ( 'NONE',  ( -0.1181102362204723977, 2.444206406002937815, -0.03937007874015747977 ) ) ;
#11923 = CARTESIAN_POINT ( 'NONE',  ( -1.941333777923719639, -2.904294378039212976, 0.1187681980620380745 ) ) ;
#11924 = CARTESIAN_POINT ( 'NONE',  ( 7.328595018519593763E-17, 0.5905511811023621549, 0.5984251968503937480 ) ) ;
#11925 = CIRCLE ( 'NONE', #6377, 0.003937007874015749712 ) ;
#11926 = CARTESIAN_POINT ( 'NONE',  ( -1.932500704111168366, -2.783628473676827753, 0.1565635629552918073 ) ) ;
#11927 = EDGE_CURVE ( 'NONE', #6772, #9358, #1588, .T. ) ;
#11928 = ORIENTED_EDGE ( 'NONE', *, *, #5100, .F. ) ;
#11929 = CARTESIAN_POINT ( 'NONE',  ( -2.007203421661559961, -2.769453616915882321, -0.1575868804561089964 ) ) ;
#11930 = DIRECTION ( 'NONE',  ( 0.000000000000000000, 0.000000000000000000, 1.000000000000000000 ) ) ;
#11931 = FACE_OUTER_BOUND ( 'NONE', #6294, .T. ) ;
#11932 = ORIENTED_EDGE ( 'NONE', *, *, #12859, .F. ) ;
#11933 = ADVANCED_FACE ( 'NONE', ( #1366 ), #13343, .T. ) ;
#11934 = CIRCLE ( 'NONE', #2679, 0.003937007874015721089 ) ;
#11935 = ORIENTED_EDGE ( 'NONE', *, *, #13651, .T. ) ;
#11936 = ORIENTED_EDGE ( 'NONE', *, *, #5167, .F. ) ;
#11937 = AXIS2_PLACEMENT_3D ( 'NONE', #11541, #10686, #10363 ) ;
#11938 = DIRECTION ( 'NONE',  ( 0.000000000000000000, 0.000000000000000000, -1.000000000000000000 ) ) ;
#11939 = DIRECTION ( 'NONE',  ( -0.000000000000000000, -1.000000000000000000, -0.000000000000000000 ) ) ;
#11940 = CARTESIAN_POINT ( 'NONE',  ( 0.000000000000000000, 1.370078740157480546, 0.000000000000000000 ) ) ;
#11941 = CARTESIAN_POINT ( 'NONE',  ( 0.000000000000000000, 0.06496062992125986590, 0.000000000000000000 ) ) ;
#11942 = CONTEXT_DEPENDENT_SHAPE_REPRESENTATION ( #303, #11190 ) ;
#11943 = DIRECTION ( 'NONE',  ( -0.3445509047204711184, -0.9387676358163955515, 0.000000000000000000 ) ) ;
#11944 = CIRCLE ( 'NONE', #10432, 0.7086614173228346081 ) ;
#11945 = CARTESIAN_POINT ( 'NONE',  ( -0.06956272065387625325, 0.1654544434110864770, -0.03844121289758908183 ) ) ;
#11946 = ORIENTED_EDGE ( 'NONE', *, *, #9033, .F. ) ;
#11947 = CYLINDRICAL_SURFACE ( 'NONE', #2670, 0.003937007874015721089 ) ;
#11948 = CARTESIAN_POINT ( 'NONE',  ( -0.2681506793016945611, -0.4921259842519685179, 0.03207310886158504931 ) ) ;
#11949 = VECTOR ( 'NONE', #12935, 39.37007874015748143 ) ;
#11950 = DIRECTION ( 'NONE',  ( 0.8660254037844389297, 0.000000000000000000, -0.4999999999999994449 ) ) ;
#11951 = EDGE_CURVE ( 'NONE', #11465, #5753, #9763, .T. ) ;
#11952 = DIRECTION ( 'NONE',  ( -0.000000000000000000, -1.000000000000000000, -0.000000000000000000 ) ) ;
#11953 = EDGE_CURVE ( 'NONE', #731, #12158, #8083, .T. ) ;
#11954 = CIRCLE ( 'NONE', #440, 0.7007874015748031260 ) ;
#11955 = EDGE_LOOP ( 'NONE', ( #8433, #2310, #743, #9241 ) ) ;
#11956 = VERTEX_POINT ( 'NONE', #8560 ) ;
#11957 = ORIENTED_EDGE ( 'NONE', *, *, #6563, .T. ) ;
#11958 = AXIS2_PLACEMENT_3D ( 'NONE', #5714, #6900, #10509 ) ;
#11959 = ORIENTED_EDGE ( 'NONE', *, *, #15146, .T. ) ;
#11960 = ADVANCED_FACE ( 'NONE', ( #8796 ), #14875, .T. ) ;
#11961 = ORIENTED_EDGE ( 'NONE', *, *, #9065, .F. ) ;
#11962 = CYLINDRICAL_SURFACE ( 'NONE', #10143, 0.003937007874015721089 ) ;
#11963 = LINE ( 'NONE', #1225, #5830 ) ;
#11964 = CARTESIAN_POINT ( 'NONE',  ( 0.4783464566929142014, -0.4881889763779528324, 0.3534565624369548908 ) ) ;
#11965 = DIRECTION ( 'NONE',  ( 1.961103758713082858E-16, 0.9885803249658942082, 0.1506948608623633334 ) ) ;
#11966 = CYLINDRICAL_SURFACE ( 'NONE', #14616, 0.03937007874015759773 ) ;
#11967 = DIRECTION ( 'NONE',  ( -0.000000000000000000, -1.000000000000000000, -0.000000000000000000 ) ) ;
#11968 = DIRECTION ( 'NONE',  ( -1.000000000000000000, 0.000000000000000000, 0.000000000000000000 ) ) ;
#11969 = DIRECTION ( 'NONE',  ( -0.000000000000000000, -1.000000000000000000, -0.000000000000000000 ) ) ;
#11970 = CARTESIAN_POINT ( 'NONE',  ( 0.5894146648244296127, -0.09448818897637796532, 0.1610807828475372405 ) ) ;
#11971 = CIRCLE ( 'NONE', #9962, 0.03937007874015761855 ) ;
#11972 = B_SPLINE_CURVE_WITH_KNOTS ( 'NONE', 3,
 ( #6175, #11929, #4709, #3606, #8302, #7277, #12236, #3827, #13077, #2664, #9496, #8531, #10737, #14335, #5001, #7128, #1195, #5948, #8386, #8611, #2343, #13170, #9796, #1261, #18, #3690, #10967, #10887, #178, #9730, #6088, #13397, #7436, #9652, #7213, #4778, #14266, #5864, #9563, #2434 ),
 .UNSPECIFIED., .F., .F.,
 ( 4, 2, 2, 2, 2, 2, 2, 2, 2, 2, 2, 2, 2, 2, 2, 2, 2, 2, 2, 4 ),
 ( 0.000000000000000000, 0.0008795077490859314886, 0.001759015498171862977, 0.002638523247257794357, 0.003518030996343725954, 0.004397538745429656684, 0.004837292619972635710, 0.005277046494515613868, 0.005716800369058592027, 0.006156554243601570185, 0.007036061992687516094, 0.007475815867230489915, 0.007915569741773462870, 0.008795077490859405309, 0.009674585239945351217, 0.01055409298903129539, 0.01143360073811723783, 0.01231310848720318200, 0.01319261623628912618, 0.01407212398537507209 ),
 .UNSPECIFIED. ) ;
#11973 = CARTESIAN_POINT ( 'NONE',  ( -1.084824920504545016E-17, 0.000000000000000000, -0.08858267716535432601 ) ) ;
#11974 = DIRECTION ( 'NONE',  ( 0.000000000000000000, -1.000000000000000000, 0.000000000000000000 ) ) ;
#11975 = AXIS2_PLACEMENT_3D ( 'NONE', #2226, #11715, #981 ) ;
#11976 = ORIENTED_EDGE ( 'NONE', *, *, #9854, .F. ) ;
#11977 = ORIENTED_EDGE ( 'NONE', *, *, #12527, .T. ) ;
#11978 = ORIENTED_EDGE ( 'NONE', *, *, #8490, .T. ) ;
#11979 = ORIENTED_EDGE ( 'NONE', *, *, #14195, .F. ) ;
#11980 = EDGE_CURVE ( 'NONE', #5700, #9010, #7469, .T. ) ;
#11981 = CIRCLE ( 'NONE', #9727, 0.003937007874015758385 ) ;
#11982 = CARTESIAN_POINT ( 'NONE',  ( -2.107032882782853722, -1.725908548393271458, -0.1037381152052583161 ) ) ;
#11983 = CARTESIAN_POINT ( 'NONE',  ( 0.2681506793018588186, -0.4881889763779528324, 0.03207310886168001501 ) ) ;
#11984 = CIRCLE ( 'NONE', #12872, 0.003937007874015749712 ) ;
#11985 = CARTESIAN_POINT ( 'NONE',  ( -0.5452492930724200937, 1.338582677165354395, 0.2466088494548780152 ) ) ;
#11986 = DIRECTION ( 'NONE',  ( -0.000000000000000000, -0.000000000000000000, -1.000000000000000000 ) ) ;
#11987 = CARTESIAN_POINT ( 'NONE',  ( 7.328595018519593763E-17, 1.661417322834646049, 0.5984251968503937480 ) ) ;
#11988 = CARTESIAN_POINT ( 'NONE',  ( -0.06299212598414161146, -0.4921259842519685179, -0.5909884645248154600 ) ) ;
#11989 = ORIENTED_EDGE ( 'NONE', *, *, #15276, .T. ) ;
#11990 = CARTESIAN_POINT ( 'NONE',  ( -0.1724006475077544398, -0.1023622047244094474, 0.1768186671464649640 ) ) ;
#11991 = DIRECTION ( 'NONE',  ( -3.614007241618347785E-16, 0.000000000000000000, 1.000000000000000000 ) ) ;
#11992 = CARTESIAN_POINT ( 'NONE',  ( 0.000000000000000000, 0.000000000000000000, -0.5905511811023621549 ) ) ;
#11993 = AXIS2_PLACEMENT_3D ( 'NONE', #7433, #11029, #7274 ) ;
#11994 = VERTEX_POINT ( 'NONE', #14602 ) ;
#11995 = ORIENTED_EDGE ( 'NONE', *, *, #3861, .T. ) ;
#11996 = ORIENTED_EDGE ( 'NONE', *, *, #4787, .T. ) ;
#11997 = EDGE_CURVE ( 'NONE', #9448, #12429, #618, .T. ) ;
#11998 = FACE_BOUND ( 'NONE', #14507, .T. ) ;
#11999 = EDGE_CURVE ( 'NONE', #13962, #4061, #7102, .T. ) ;
#12000 = CARTESIAN_POINT ( 'NONE',  ( -0.06299212598414173636, -0.4881889763779528324, -0.2377126739438355507 ) ) ;
#12001 = FACE_OUTER_BOUND ( 'NONE', #14436, .T. ) ;
#12002 = CARTESIAN_POINT ( 'NONE',  ( 0.000000000000000000, 0.3543307086614172485, 0.000000000000000000 ) ) ;
#12003 = CARTESIAN_POINT ( 'NONE',  ( 0.1872249459501148516, -0.09842519685039370636, -0.1080943729433118949 ) ) ;
#12004 = EDGE_LOOP ( 'NONE', ( #5536, #12694, #14555 ) ) ;
#12005 = FACE_OUTER_BOUND ( 'NONE', #3641, .T. ) ;
#12006 = CARTESIAN_POINT ( 'NONE',  ( 0.5418660417173575272, -0.4921259842519685179, 0.2355633981508976349 ) ) ;
#12007 = CARTESIAN_POINT ( 'NONE',  ( -0.07874015748031520934, 1.062385330869439640E-16, 0.01968503937007873988 ) ) ;
#12008 = ORIENTED_EDGE ( 'NONE', *, *, #4046, .F. ) ;
#12009 = VERTEX_POINT ( 'NONE', #13271 ) ;
#12010 = EDGE_CURVE ( 'NONE', #12092, #8855, #9114, .T. ) ;
#12011 = ORIENTED_EDGE ( 'NONE', *, *, #14417, .F. ) ;
#12012 = EDGE_CURVE ( 'NONE', #1879, #12256, #12362, .T. ) ;
#12013 = LINE ( 'NONE', #1273, #10827 ) ;
#12014 = ADVANCED_FACE ( 'NONE', ( #12325 ), #13564, .F. ) ;
#12015 = DIRECTION ( 'NONE',  ( -0.000000000000000000, -1.000000000000000000, -0.000000000000000000 ) ) ;
#12016 = CARTESIAN_POINT ( 'NONE',  ( 0.000000000000000000, -0.09842519685039370636, 0.000000000000000000 ) ) ;
#12017 = DIRECTION ( 'NONE',  ( -1.000000000000000000, -0.000000000000000000, -0.000000000000000000 ) ) ;
#12018 = DIRECTION ( 'NONE',  ( 1.000000000000000000, 0.000000000000000000, 0.000000000000000000 ) ) ;
#12019 = CARTESIAN_POINT ( 'NONE',  ( 0.000000000000000000, 2.165354330708661568, 0.1535433070866141780 ) ) ;
#12020 = ORIENTED_EDGE ( 'NONE', *, *, #10985, .T. ) ;
#12021 = FACE_OUTER_BOUND ( 'NONE', #8848, .T. ) ;
#12022 = DIRECTION ( 'NONE',  ( 1.000000000000000000, 0.000000000000000000, 0.000000000000000000 ) ) ;
#12023 = CARTESIAN_POINT ( 'NONE',  ( -0.07874015748031543138, -0.1682792322177920907, 0.05905511811023622659 ) ) ;
#12024 = CARTESIAN_POINT ( 'NONE',  ( 0.4591888763630541104, -0.4881889763779528324, 0.3787644491703230365 ) ) ;
#12025 = ORIENTED_EDGE ( 'NONE', *, *, #6368, .T. ) ;
#12026 = EDGE_CURVE ( 'NONE', #11417, #9358, #124, .T. ) ;
#12027 = ORIENTED_EDGE ( 'NONE', *, *, #2960, .T. ) ;
#12028 = EDGE_CURVE ( 'NONE', #1797, #9820, #6095, .T. ) ;
#12029 = ORIENTED_EDGE ( 'NONE', *, *, #12633, .F. ) ;
#12030 = FACE_BOUND ( 'NONE', #4045, .T. ) ;
#12031 = ADVANCED_FACE ( 'NONE', ( #4313 ), #14631, .T. ) ;
#12032 = DIRECTION ( 'NONE',  ( -0.000000000000000000, 0.000000000000000000, 1.000000000000000000 ) ) ;
#12033 = CARTESIAN_POINT ( 'NONE',  ( -1.914091141911949734, -2.904218397859934075, 0.1188472834034596526 ) ) ;
#12034 = CARTESIAN_POINT ( 'NONE',  ( 0.08858267716532777780, 36.23251143493369142, -1.111019662821471021 ) ) ;
#12035 = DIRECTION ( 'NONE',  ( 0.8660254037844501429, 0.000000000000000000, 0.4999999999999798495 ) ) ;
#12036 = CARTESIAN_POINT ( 'NONE',  ( -2.184126211765464287, -1.693613514254873165, 0.08383392658276944687 ) ) ;
#12037 = CARTESIAN_POINT ( 'NONE',  ( 0.3117681530218320840, -0.2952755905511811330, 0.2981971199768684855 ) ) ;
#12038 = CARTESIAN_POINT ( 'NONE',  ( 0.000000000000000000, 0.03937007874015749365, 0.000000000000000000 ) ) ;
#12039 = EDGE_CURVE ( 'NONE', #1202, #11305, #1363, .T. ) ;
#12040 = CARTESIAN_POINT ( 'NONE',  ( -0.5450083523900178806, 1.043307086614173373, 0.2464697422870344157 ) ) ;
#12041 = DIRECTION ( 'NONE',  ( -0.4999999999999967248, -4.336808689941996437E-15, -0.8660254037844405950 ) ) ;
#12042 = EDGE_LOOP ( 'NONE', ( #8277, #1762, #14758, #6599 ) ) ;
#12043 = ORIENTED_EDGE ( 'NONE', *, *, #10545, .T. ) ;
#12044 = VERTEX_POINT ( 'NONE', #4094 ) ;
#12045 = CARTESIAN_POINT ( 'NONE',  ( 0.05905511811023622659, 1.190944881889763884, -0.8661417322834648047 ) ) ;
#12046 = CARTESIAN_POINT ( 'NONE',  ( -0.2755905511811023167, -0.02638708502139245488, -0.03937007874015747977 ) ) ;
#12047 = EDGE_CURVE ( 'NONE', #4812, #13356, #1131, .T. ) ;
#12048 = CARTESIAN_POINT ( 'NONE',  ( 0.1023622047244638067, -0.4881889763779528324, -0.2482618547481154347 ) ) ;
#12049 = CARTESIAN_POINT ( 'NONE',  ( 0.05905511811023622659, 1.190944881889763884, -0.8267716535433072833 ) ) ;
#12050 = DIRECTION ( 'NONE',  ( -0.8660254037844385966, 0.000000000000000000, 0.5000000000000001110 ) ) ;
#12051 = DIRECTION ( 'NONE',  ( -0.8660254037844381525, 0.000000000000000000, 0.5000000000000006661 ) ) ;
#12052 = ADVANCED_FACE ( 'NONE', ( #4407 ), #2851, .T. ) ;
#12053 = LINE ( 'NONE', #9547, #9454 ) ;
#12054 = EDGE_CURVE ( 'NONE', #13558, #5085, #3239, .T. ) ;
#12055 = DIRECTION ( 'NONE',  ( -1.000000000000000000, -0.000000000000000000, -3.614007241618347785E-16 ) ) ;
#12056 = LINE ( 'NONE', #157, #13162 ) ;
#12057 = VERTEX_POINT ( 'NONE', #2931 ) ;
#12058 = VERTEX_POINT ( 'NONE', #1751 ) ;
#12059 = VERTEX_POINT ( 'NONE', #13888 ) ;
#12060 = CARTESIAN_POINT ( 'NONE',  ( -1.293236445124221312, 0.1355266887446167634, -0.03937007874015747977 ) ) ;
#12061 = CARTESIAN_POINT ( 'NONE',  ( 0.02952755905511747145, -0.09842519685039370636, 0.05114323250695394785 ) ) ;
#12062 = CARTESIAN_POINT ( 'NONE',  ( -1.452763252956529083, -0.05091287232363069654, -0.1033464566929133133 ) ) ;
#12063 = CARTESIAN_POINT ( 'NONE',  ( -2.011807227224586825, -2.756102811318747126, 0.1765457041329571430 ) ) ;
#12064 = CARTESIAN_POINT ( 'NONE',  ( 0.06440205152079661599, 1.037100910086407257, -0.5870313606185345590 ) ) ;
#12065 = CARTESIAN_POINT ( 'NONE',  ( -1.915575942926155406, -2.830573451792969486, 0.1438162775209220201 ) ) ;
#12066 = ORIENTED_EDGE ( 'NONE', *, *, #14856, .T. ) ;
#12067 = CYLINDRICAL_SURFACE ( 'NONE', #436, 0.003937007874015741038 ) ;
#12068 = CARTESIAN_POINT ( 'NONE',  ( -0.008251140381529230641, 0.1525182358981297670, -0.01646613645217641364 ) ) ;
#12069 = ORIENTED_EDGE ( 'NONE', *, *, #8063, .T. ) ;
#12070 = ORIENTED_EDGE ( 'NONE', *, *, #12047, .T. ) ;
#12071 = UNCERTAINTY_MEASURE_WITH_UNIT (LENGTH_MEASURE( 1.000000000000000082E-05 ), #14065, 'distance_accuracy_value', 'NONE');
#12072 = ORIENTED_EDGE ( 'NONE', *, *, #6655, .T. ) ;
#12073 = DIRECTION ( 'NONE',  ( -0.5000000000000004441, -1.618519037356983674E-14, -0.8660254037844383745 ) ) ;
#12074 = DIRECTION ( 'NONE',  ( 0.8660254037844383745, 0.000000000000000000, -0.5000000000000004441 ) ) ;
#12075 = CYLINDRICAL_SURFACE ( 'NONE', #2357, 0.5511811023622046335 ) ;
#12076 = FACE_OUTER_BOUND ( 'NONE', #4304, .T. ) ;
#12077 = DIRECTION ( 'NONE',  ( 0.000000000000000000, 0.000000000000000000, 1.000000000000000000 ) ) ;
#12078 = CARTESIAN_POINT ( 'NONE',  ( -1.180847381051866485, 0.3433074774306730803, 0.03937007874015747977 ) ) ;
#12079 = ORIENTED_EDGE ( 'NONE', *, *, #14812, .F. ) ;
#12080 = EDGE_CURVE ( 'NONE', #3171, #11605, #857, .T. ) ;
#12081 = DIRECTION ( 'NONE',  ( -1.000000000000000000, 0.000000000000000000, 0.000000000000000000 ) ) ;
#12082 = DIRECTION ( 'NONE',  ( 0.000000000000000000, -1.000000000000000000, 0.000000000000000000 ) ) ;
#12083 = CARTESIAN_POINT ( 'NONE',  ( -0.3944453183761345572, -0.2952755905511811330, 0.1549960689574421957 ) ) ;
#12084 = CIRCLE ( 'NONE', #2077, 0.03937007874015751446 ) ;
#12085 = CARTESIAN_POINT ( 'NONE',  ( -0.1618514667033795484, -0.09842519685039370636, 0.2161887458866224576 ) ) ;
#12086 = ADVANCED_FACE ( 'NONE', ( #6507 ), #803, .T. ) ;
#12087 = TOROIDAL_SURFACE ( 'NONE', #12337, 0.04330708661417328326, 0.003937007874015747977 ) ;
#12088 = PRESENTATION_STYLE_ASSIGNMENT (( #2597 ) ) ;
#12089 = ORIENTED_EDGE ( 'NONE', *, *, #5058, .T. ) ;
#12090 = EDGE_CURVE ( 'NONE', #1174, #1730, #11617, .T. ) ;
#12091 = ORIENTED_EDGE ( 'NONE', *, *, #6721, .T. ) ;
#12092 = VERTEX_POINT ( 'NONE', #7849 ) ;
#12093 = VERTEX_POINT ( 'NONE', #10134 ) ;
#12094 = LINE ( 'NONE', #275, #14914 ) ;
#12095 = TOROIDAL_SURFACE ( 'NONE', #3086, 0.6614173228346456046, 0.007874015748031495954 ) ;
#12096 = CIRCLE ( 'NONE', #8850, 0.03937007874015751446 ) ;
#12097 = TOROIDAL_SURFACE ( 'NONE', #8588, 0.5984251968503937480, 0.007874015748031495954 ) ;
#12098 = CARTESIAN_POINT ( 'NONE',  ( 0.5860051159906326523, -0.09842519685039370636, 0.1591122789105293422 ) ) ;
#12099 = DIRECTION ( 'NONE',  ( 0.000000000000000000, 1.000000000000000000, 0.000000000000000000 ) ) ;
#12100 = CIRCLE ( 'NONE', #1335, 0.2362204724409449619 ) ;
#12101 = CARTESIAN_POINT ( 'NONE',  ( 0.8045879322627373931, 37.37889961492984270, 0.2599561292507698296 ) ) ;
#12102 = CARTESIAN_POINT ( 'NONE',  ( -1.398125690441303526, -0.003404927804347070153, 0.05905511811023622659 ) ) ;
#12103 = CARTESIAN_POINT ( 'NONE',  ( -2.090051324975654268, -1.858423098537180129, 0.1968503937007874127 ) ) ;
#12104 = DIRECTION ( 'NONE',  ( 1.000000000000000000, 0.000000000000000000, 0.000000000000000000 ) ) ;
#12105 = SHAPE_REPRESENTATION ( 'Finger', ( #11481 ), #9487 ) ;
#12106 = CARTESIAN_POINT ( 'NONE',  ( 0.000000000000000000, 1.035433070866141891, -0.5905511811023621549 ) ) ;
#12107 = ADVANCED_FACE ( 'NONE', ( #8971 ), #10217, .F. ) ;
#12108 =( REPRESENTATION_RELATIONSHIP ('NONE','NONE', #8904, #12705 ) REPRESENTATION_RELATIONSHIP_WITH_TRANSFORMATION ( #5795 )SHAPE_REPRESENTATION_RELATIONSHIP( ) );
#12109 = DIRECTION ( 'NONE',  ( 1.000000000000000000, 0.000000000000000000, 0.000000000000000000 ) ) ;
#12110 = CARTESIAN_POINT ( 'NONE',  ( 0.1213717603336464113, 2.440944881889763884, 0.04263160285333146560 ) ) ;
#12111 = AXIS2_PLACEMENT_3D ( 'NONE', #14847, #6602, #456 ) ;
#12112 = AXIS2_PLACEMENT_3D ( 'NONE', #4335, #13910, #14145 ) ;
#12113 = ORIENTED_EDGE ( 'NONE', *, *, #3396, .T. ) ;
#12114 = AXIS2_PLACEMENT_3D ( 'NONE', #6415, #7449, #11208 ) ;
#12115 = EDGE_CURVE ( 'NONE', #8036, #1499, #6597, .T. ) ;
#12116 = AXIS2_PLACEMENT_3D ( 'NONE', #439, #2938, #14770 ) ;
#12117 = ORIENTED_EDGE ( 'NONE', *, *, #9273, .T. ) ;
#12118 = VERTEX_POINT ( 'NONE', #15144 ) ;
#12119 = CARTESIAN_POINT ( 'NONE',  ( 0.000000000000000000, 0.5984251968503937480, -0.5984251968503937480 ) ) ;
#12120 = DIRECTION ( 'NONE',  ( 0.000000000000000000, 0.000000000000000000, 1.000000000000000000 ) ) ;
#12121 = AXIS2_PLACEMENT_3D ( 'NONE', #5526, #5611, #9235 ) ;
#12122 = DIRECTION ( 'NONE',  ( -1.000000000000000000, 0.000000000000000000, 0.000000000000000000 ) ) ;
#12123 = AXIS2_PLACEMENT_3D ( 'NONE', #3173, #5805, #8261 ) ;
#12124 = AXIS2_PLACEMENT_3D ( 'NONE', #4840, #13006, #2267 ) ;
#12125 = PLANE ( 'NONE',  #13657 ) ;
#12126 = AXIS2_PLACEMENT_3D ( 'NONE', #15360, #15447, #12936 ) ;
#12127 = DIRECTION ( 'NONE',  ( 0.6421085279136217183, 0.7666137478421592988, -1.662328581735447640E-15 ) ) ;
#12128 = AXIS2_PLACEMENT_3D ( 'NONE', #3951, #9986, #8729 ) ;
#12129 = DIRECTION ( 'NONE',  ( 0.000000000000000000, -1.000000000000000000, 2.212657494868377674E-16 ) ) ;
#12130 = AXIS2_PLACEMENT_3D ( 'NONE', #3558, #7243, #2386 ) ;
#12131 = CARTESIAN_POINT ( 'NONE',  ( 0.06767366483286080259, -0.2952755905511811330, 0.7209811753676967916 ) ) ;
#12132 = LINE ( 'NONE', #9710, #13084 ) ;
#12133 = CARTESIAN_POINT ( 'NONE',  ( 0.4815353412745266848, 1.340095897400991554, 0.3474236500605469291 ) ) ;
#12134 = EDGE_LOOP ( 'NONE', ( #7435, #15104, #4985, #8093 ) ) ;
#12135 = ORIENTED_EDGE ( 'NONE', *, *, #13737, .T. ) ;
#12136 = ADVANCED_FACE ( 'NONE', ( #1817 ), #507, .F. ) ;
#12137 = AXIS2_PLACEMENT_3D ( 'NONE', #1278, #7368, #1211 ) ;
#12138 = CIRCLE ( 'NONE', #4905, 0.007874015748031449116 ) ;
#12139 = ORIENTED_EDGE ( 'NONE', *, *, #12484, .T. ) ;
#12140 = CIRCLE ( 'NONE', #5858, 0.05905511811023627516 ) ;
#12141 = CIRCLE ( 'NONE', #2358, 0.003937007874015724558 ) ;
#12142 = ORIENTED_EDGE ( 'NONE', *, *, #13797, .F. ) ;
#12143 = AXIS2_PLACEMENT_3D ( 'NONE', #14512, #8542, #9889 ) ;
#12144 = DIRECTION ( 'NONE',  ( 0.000000000000000000, 0.000000000000000000, -1.000000000000000000 ) ) ;
#12145 = ADVANCED_FACE ( 'NONE', ( #13808 ), #13610, .F. ) ;
#12146 = FACE_OUTER_BOUND ( 'NONE', #357, .T. ) ;
#12147 = CARTESIAN_POINT ( 'NONE',  ( -1.551763806551527347, 0.1400464552716836897, 0.05905511811023622659 ) ) ;
#12148 = CARTESIAN_POINT ( 'NONE',  ( -2.182693454834260027, -1.630005269948474167, 0.1033464566929130080 ) ) ;
#12149 = CIRCLE ( 'NONE', #11641, 0.5905511811023621549 ) ;
#12150 = DIRECTION ( 'NONE',  ( 1.000000000000000000, -8.673617379884049672E-15, 0.000000000000000000 ) ) ;
#12151 = AXIS2_PLACEMENT_3D ( 'NONE', #7981, #15194, #7598 ) ;
#12152 = CARTESIAN_POINT ( 'NONE',  ( -1.941813874431828957, -2.756691771901667476, 0.1575933035815317296 ) ) ;
#12153 = CIRCLE ( 'NONE', #8894, 0.003937007874015737569 ) ;
#12154 = ORIENTED_EDGE ( 'NONE', *, *, #15399, .T. ) ;
#12155 = DIRECTION ( 'NONE',  ( 0.5000000000000037748, -0.000000000000000000, 0.8660254037844365982 ) ) ;
#12156 = DIRECTION ( 'NONE',  ( 1.243449787580175325E-14, 4.625929269271485914E-16, 1.000000000000000000 ) ) ;
#12157 = CARTESIAN_POINT ( 'NONE',  ( 0.09842519685044820443, -0.4921259842519685179, -0.5870514566507987197 ) ) ;
#12158 = VERTEX_POINT ( 'NONE', #7936 ) ;
#12159 = EDGE_LOOP ( 'NONE', ( #6201, #679, #15177, #4735 ) ) ;
#12161 = VERTEX_POINT ( 'NONE', #12729 ) ;
#12160 = AXIS2_PLACEMENT_3D ( 'NONE', #2864, #13454, #11250 ) ;
#12162 = ORIENTED_EDGE ( 'NONE', *, *, #4067, .F. ) ;
#12163 = DIRECTION ( 'NONE',  ( 0.000000000000000000, 0.000000000000000000, -1.000000000000000000 ) ) ;
#12164 = CARTESIAN_POINT ( 'NONE',  ( 0.000000000000000000, -0.09842519685039370636, 0.2161887458866224576 ) ) ;
#12165 = CARTESIAN_POINT ( 'NONE',  ( 0.4815353412745266848, 1.340095897400991554, 0.3474236500605469291 ) ) ;
#12166 = DIRECTION ( 'NONE',  ( 1.224646799147353207E-16, 0.000000000000000000, -1.000000000000000000 ) ) ;
#12167 = DIRECTION ( 'NONE',  ( -0.000000000000000000, -1.000000000000000000, -0.000000000000000000 ) ) ;
#12168 = CYLINDRICAL_SURFACE ( 'NONE', #627, 0.003937007874015749712 ) ;
#12169 = VERTEX_POINT ( 'NONE', #1988 ) ;
#12170 = PLANE ( 'NONE',  #13431 ) ;
#12171 = CARTESIAN_POINT ( 'NONE',  ( 0.1574803149606299191, -0.003937007874015747977, -0.5909884645248143498 ) ) ;
#12172 = CARTESIAN_POINT ( 'NONE',  ( -1.190198933766853706, 0.3259758027579612860, -0.05905511811023622659 ) ) ;
#12173 = VECTOR ( 'NONE', #10350, 39.37007874015748854 ) ;
#12174 = AXIS2_PLACEMENT_3D ( 'NONE', #14550, #8753, #1399 ) ;
#12175 = DIRECTION ( 'NONE',  ( 0.8660254037844365982, -0.000000000000000000, 0.5000000000000035527 ) ) ;
#12176 = CARTESIAN_POINT ( 'NONE',  ( 5.303588500244447761E-18, 0.07480314960629921850, -0.04330708661417326938 ) ) ;
#12177 = AXIS2_PLACEMENT_3D ( 'NONE', #3730, #13275, #8657 ) ;
#12178 = ORIENTED_EDGE ( 'NONE', *, *, #2264, .T. ) ;
#12179 = EDGE_LOOP ( 'NONE', ( #13943, #2246, #14954, #7654 ) ) ;
#12180 = ORIENTED_EDGE ( 'NONE', *, *, #10181, .T. ) ;
#12181 = EDGE_LOOP ( 'NONE', ( #2466, #7733, #8616, #12943, #12802, #9566, #4512 ) ) ;
#12182 = EDGE_CURVE ( 'NONE', #315, #7883, #1864, .T. ) ;
#12183 = FACE_OUTER_BOUND ( 'NONE', #7903, .T. ) ;
#12184 = DIRECTION ( 'NONE',  ( 0.5750876580239430158, 0.8180917953313895374, 0.000000000000000000 ) ) ;
#12185 = AXIS2_PLACEMENT_3D ( 'NONE', #12652, #7857, #11301 ) ;
#12186 = EDGE_CURVE ( 'NONE', #9296, #749, #9623, .T. ) ;
#12187 = DIRECTION ( 'NONE',  ( 0.000000000000000000, 1.000000000000000000, -0.000000000000000000 ) ) ;
#12188 = CARTESIAN_POINT ( 'NONE',  ( -0.5418660417173573052, -0.4881889763779528324, 0.2355633981508970520 ) ) ;
#12189 = DIRECTION ( 'NONE',  ( 0.7484559191945135970, 0.5030755238499722282, -0.4321212264235256839 ) ) ;
#12190 = VECTOR ( 'NONE', #11362, 39.37007874015748143 ) ;
#12191 = CYLINDRICAL_SURFACE ( 'NONE', #5350, 0.007874015748031482076 ) ;
#12192 = CARTESIAN_POINT ( 'NONE',  ( 8.100026073100603114E-17, 0.5433070866141731514, -0.6614173228346456046 ) ) ;
#12193 = EDGE_CURVE ( 'NONE', #15270, #381, #13092, .T. ) ;
#12194 = DIRECTION ( 'NONE',  ( -0.000000000000000000, -1.000000000000000000, -0.000000000000000000 ) ) ;
#12195 = DIRECTION ( 'NONE',  ( 0.4999999999999998335, 0.000000000000000000, 0.8660254037844388186 ) ) ;
#12196 = FACE_BOUND ( 'NONE', #10627, .T. ) ;
#12197 = AXIS2_PLACEMENT_3D ( 'NONE', #876, #9422, #13964 ) ;
#12198 = EDGE_LOOP ( 'NONE', ( #14952, #15311, #13402, #4693 ) ) ;
#12199 = ORIENTED_EDGE ( 'NONE', *, *, #3802, .F. ) ;
#12200 = AXIS2_PLACEMENT_3D ( 'NONE', #14013, #10413, #4457 ) ;
#12201 = VERTEX_POINT ( 'NONE', #2286 ) ;
#12202 = ADVANCED_FACE ( 'NONE', ( #7060 ), #11705, .T. ) ;
#12203 = CIRCLE ( 'NONE', #2191, 0.03937007874015751446 ) ;
#12204 = ADVANCED_FACE ( 'NONE', ( #13023 ), #1608, .T. ) ;
#12205 = CARTESIAN_POINT ( 'NONE',  ( -2.100298540928004165, -2.106218814929184724, -0.1158686206437609667 ) ) ;
#12206 = CARTESIAN_POINT ( 'NONE',  ( -1.943704794560271676, -2.936197138332786061, -0.06765823053126623909 ) ) ;
#12207 = DIRECTION ( 'NONE',  ( 0.000000000000000000, 0.000000000000000000, 1.000000000000000000 ) ) ;
#12208 = AXIS2_PLACEMENT_3D ( 'NONE', #2125, #6807, #8068 ) ;
#12209 = CARTESIAN_POINT ( 'NONE',  ( 0.5576140732134206024, -0.09842519685039370636, 0.2082870074805215910 ) ) ;
#12210 = EDGE_CURVE ( 'NONE', #9354, #15234, #9044, .T. ) ;
#12211 = DIRECTION ( 'NONE',  ( 0.000000000000000000, 1.000000000000000000, 0.000000000000000000 ) ) ;
#12212 = CARTESIAN_POINT ( 'NONE',  ( 0.000000000000000000, 0.000000000000000000, -0.5511811023622046335 ) ) ;
#12213 = VECTOR ( 'NONE', #267, 39.37007874015748143 ) ;
#12214 = CARTESIAN_POINT ( 'NONE',  ( -0.02641567992992046449, 0.1724028871747071145, 1.853431881210122409E-17 ) ) ;
#12215 = CARTESIAN_POINT ( 'NONE',  ( -0.002500327830563135300, -0.1654030484222656916, 8.530201525337163767E-32 ) ) ;
#12216 = CARTESIAN_POINT ( 'NONE',  ( 0.06604848736013260724, 1.346456692913385877, -0.5868460571724354313 ) ) ;
#12217 = DIRECTION ( 'NONE',  ( -0.000000000000000000, -2.212657494868377674E-16, 1.000000000000000000 ) ) ;
#12218 = ORIENTED_EDGE ( 'NONE', *, *, #9029, .T. ) ;
#12219 = VERTEX_POINT ( 'NONE', #10444 ) ;
#12220 = CIRCLE ( 'NONE', #6683, 0.1240157480314959260 ) ;
#12221 = VERTEX_POINT ( 'NONE', #9509 ) ;
#12222 = ORIENTED_EDGE ( 'NONE', *, *, #13057, .F. ) ;
#12223 = ORIENTED_EDGE ( 'NONE', *, *, #6677, .F. ) ;
#12224 = AXIS2_PLACEMENT_3D ( 'NONE', #10667, #6736, #4711 ) ;
#12225 = EDGE_CURVE ( 'NONE', #631, #8019, #14045, .T. ) ;
#12226 = CARTESIAN_POINT ( 'NONE',  ( -1.419105553176674306, -0.01195146698575283613, -0.07341972397144938545 ) ) ;
#12227 = DIRECTION ( 'NONE',  ( 1.000000000000000000, 0.000000000000000000, 0.000000000000000000 ) ) ;
#12228 = EDGE_CURVE ( 'NONE', #3506, #5345, #10359, .T. ) ;
#12229 = CARTESIAN_POINT ( 'NONE',  ( 1.181102362204724310, 4.044111181948214319E-16, -0.02559055118110236185 ) ) ;
#12230 = EDGE_CURVE ( 'NONE', #4739, #4286, #1077, .T. ) ;
#12231 = FACE_OUTER_BOUND ( 'NONE', #6144, .T. ) ;
#12233 = AXIS2_PLACEMENT_3D ( 'NONE', #723, #1803, #643 ) ;
#12232 = FACE_BOUND ( 'NONE', #1022, .T. ) ;
#12234 = CARTESIAN_POINT ( 'NONE',  ( -1.868651797801601733, -2.949104743336227408, -0.01367295599960066839 ) ) ;
#12235 = ORIENTED_EDGE ( 'NONE', *, *, #13719, .T. ) ;
#12236 = CARTESIAN_POINT ( 'NONE',  ( -1.980110816268535689, -2.844065425694749738, -0.1439511263496600080 ) ) ;
#12237 = DIRECTION ( 'NONE',  ( -6.571729149350554040E-16, -5.967930543588097370E-16, 1.000000000000000000 ) ) ;
#12238 = VECTOR ( 'NONE', #291, 39.37007874015748143 ) ;
#12239 = LINE ( 'NONE', #9798, #15224 ) ;
#12240 = VERTEX_POINT ( 'NONE', #3542 ) ;
#12241 = EDGE_CURVE ( 'NONE', #6593, #1223, #7356, .T. ) ;
#12242 = ORIENTED_EDGE ( 'NONE', *, *, #3893, .T. ) ;
#12243 = ORIENTED_EDGE ( 'NONE', *, *, #6244, .F. ) ;
#12244 = CARTESIAN_POINT ( 'NONE',  ( 0.1804058482825207643, -0.4921259842519685179, -0.1041573650692960984 ) ) ;
#12245 = DIRECTION ( 'NONE',  ( 0.000000000000000000, 0.000000000000000000, 1.000000000000000000 ) ) ;
#12246 = DIRECTION ( 'NONE',  ( 0.000000000000000000, -0.000000000000000000, -1.000000000000000000 ) ) ;
#12247 = DIRECTION ( 'NONE',  ( 0.000000000000000000, -1.000000000000000000, 0.000000000000000000 ) ) ;
#12248 = CARTESIAN_POINT ( 'NONE',  ( 0.1181102362204724254, 2.448818897637795367, 0.03937007874015747977 ) ) ;
#12249 = ORIENTED_EDGE ( 'NONE', *, *, #10260, .F. ) ;
#12250 = CARTESIAN_POINT ( 'NONE',  ( 0.6864776960422569463, 1.190944881889763884, 0.4645290592786023298 ) ) ;
#12251 = DIRECTION ( 'NONE',  ( 1.349229370204184172E-15, 1.000000000000000000, -0.000000000000000000 ) ) ;
#12252 = CARTESIAN_POINT ( 'NONE',  ( 0.09948011493088554369, -0.4881889763779528324, -0.2443248468740996937 ) ) ;
#12253 = DIRECTION ( 'NONE',  ( 0.8660254037844395958, 0.000000000000000000, -0.4999999999999982236 ) ) ;
#12254 = EDGE_CURVE ( 'NONE', #10078, #12623, #10860, .T. ) ;
#12255 = VERTEX_POINT ( 'NONE', #4644 ) ;
#12256 = VERTEX_POINT ( 'NONE', #6993 ) ;
#12257 = ORIENTED_EDGE ( 'NONE', *, *, #7444, .F. ) ;
#12258 = DIRECTION ( 'NONE',  ( 0.5000000000000000000, 0.000000000000000000, 0.8660254037844388186 ) ) ;
#12259 = DIRECTION ( 'NONE',  ( 1.445602896647339903E-16, 0.000000000000000000, -1.000000000000000000 ) ) ;
#12260 = CARTESIAN_POINT ( 'NONE',  ( -1.946192867917153180, -2.743611295743889400, 0.1749236412511678829 ) ) ;
#12261 = DIRECTION ( 'NONE',  ( 0.000000000000000000, 0.000000000000000000, 1.000000000000000000 ) ) ;
#12262 = DIRECTION ( 'NONE',  ( 0.8561356751019368883, -0.1506948608623633890, -0.4942901624829528773 ) ) ;
#12263 = DIRECTION ( 'NONE',  ( -8.673617379884051249E-15, -1.000000000000000000, 0.000000000000000000 ) ) ;
#12264 = DIRECTION ( 'NONE',  ( -0.000000000000000000, -1.000000000000000000, -0.000000000000000000 ) ) ;
#12265 = CARTESIAN_POINT ( 'NONE',  ( 0.000000000000000000, -1.707404996040164512E-17, 0.000000000000000000 ) ) ;
#12266 = DIRECTION ( 'NONE',  ( -0.8660254037844309360, 0.000000000000000000, -0.5000000000000134337 ) ) ;
#12267 = CARTESIAN_POINT ( 'NONE',  ( -0.05905511811012585655, -0.09448818897637796532, -0.5909884645248143498 ) ) ;
#12268 = ORIENTED_EDGE ( 'NONE', *, *, #14113, .T. ) ;
#12269 = EDGE_LOOP ( 'NONE', ( #4354, #14491, #3738, #9964 ) ) ;
#12270 = ORIENTED_EDGE ( 'NONE', *, *, #4793, .F. ) ;
#12271 = EDGE_CURVE ( 'NONE', #2247, #8826, #4108, .T. ) ;
#12272 = DIRECTION ( 'NONE',  ( 1.000000000000000000, 0.000000000000000000, 0.000000000000000000 ) ) ;
#12273 = CARTESIAN_POINT ( 'NONE',  ( -1.933092583737872516, -2.927344828647098662, 0.08673291769302551857 ) ) ;
#12274 = CYLINDRICAL_SURFACE ( 'NONE', #3719, 0.7086614173228346081 ) ;
#12275 = LINE ( 'NONE', #3741, #9703 ) ;
#12276 = CARTESIAN_POINT ( 'NONE',  ( -1.992382107315057160, -2.749515453455444014, -0.1756903148397123415 ) ) ;
#12277 = DIRECTION ( 'NONE',  ( -0.8660254037844398178, 0.000000000000000000, 0.4999999999999979461 ) ) ;
#12278 = DIRECTION ( 'NONE',  ( -1.000000000000000000, 0.000000000000000000, 0.000000000000000000 ) ) ;
#12279 = CARTESIAN_POINT ( 'NONE',  ( -1.945459748359986252, -2.745801194614591711, 0.1561691687464105693 ) ) ;
#12280 = SPHERICAL_SURFACE ( 'NONE', #1577, 0.003937007874015747977 ) ;
#12281 = DIRECTION ( 'NONE',  ( 0.000000000000000000, 1.000000000000000000, 2.198945251238206020E-16 ) ) ;
#12282 = EDGE_CURVE ( 'NONE', #9905, #697, #8998, .T. ) ;
#12283 = ORIENTED_EDGE ( 'NONE', *, *, #3657, .T. ) ;
#12284 = ORIENTED_EDGE ( 'NONE', *, *, #2311, .F. ) ;
#12285 = ORIENTED_EDGE ( 'NONE', *, *, #2904, .T. ) ;
#12286 = ORIENTED_EDGE ( 'NONE', *, *, #116, .F. ) ;
#12287 = ADVANCED_FACE ( 'NONE', ( #6912 ), #5963, .T. ) ;
#12288 = ORIENTED_EDGE ( 'NONE', *, *, #5019, .F. ) ;
#12289 = DIRECTION ( 'NONE',  ( -1.224646799147353947E-16, 0.000000000000000000, -1.000000000000000000 ) ) ;
#12290 = CARTESIAN_POINT ( 'NONE',  ( 0.05905511811023622659, 1.190944881889763884, -0.8661417322834648047 ) ) ;
#12291 = FACE_OUTER_BOUND ( 'NONE', #4375, .T. ) ;
#12292 = CYLINDRICAL_SURFACE ( 'NONE', #4131, 0.1574803149606299191 ) ;
#12293 = CARTESIAN_POINT ( 'NONE',  ( -0.3294846884549019750, -0.2952755905511811330, 0.2675111804726950648 ) ) ;
#12294 = CARTESIAN_POINT ( 'NONE',  ( -1.190198933766852152, 0.3259758027579607864, 0.05905511811023622659 ) ) ;
#12295 = CARTESIAN_POINT ( 'NONE',  ( -1.880204665810354392, -2.921028484878219977, 0.02323882831853205100 ) ) ;
#12296 = ORIENTED_EDGE ( 'NONE', *, *, #9403, .F. ) ;
#12297 = CARTESIAN_POINT ( 'NONE',  ( 0.000000000000000000, 0.000000000000000000, 0.000000000000000000 ) ) ;
#12298 = ADVANCED_FACE ( 'NONE', ( #8313 ), #5883, .F. ) ;
#12299 = CARTESIAN_POINT ( 'NONE',  ( -1.419615703680148000, -0.01226548409420238732, -0.07587027276709679136 ) ) ;
#12300 = ADVANCED_FACE ( 'NONE', ( #3398, #4485, #9267 ), #14576, .T. ) ;
#12301 = ORIENTED_EDGE ( 'NONE', *, *, #8663, .T. ) ;
#12302 = ORIENTED_EDGE ( 'NONE', *, *, #8982, .F. ) ;
#12303 = EDGE_CURVE ( 'NONE', #5052, #10823, #6186, .T. ) ;
#12304 = ADVANCED_FACE ( 'NONE', ( #1567 ), #14369, .T. ) ;
#12305 = EDGE_LOOP ( 'NONE', ( #726, #1852, #8345 ) ) ;
#12306 = B_SPLINE_CURVE_WITH_KNOTS ( 'NONE', 3,
 ( #13876, #10123, #5314, #13649, #14909, #12717, #7834, #11456 ),
 .UNSPECIFIED., .F., .F.,
 ( 4, 2, 2, 4 ),
 ( 0.000000000000000000, 0.0007747600241158876608, 0.001162140036173831600, 0.001549520048231775322 ),
 .UNSPECIFIED. ) ;
#12307 = CARTESIAN_POINT ( 'NONE',  ( 8.678599364036360127E-17, 1.645669291338583085, 0.7086614173228346081 ) ) ;
#12308 = CARTESIAN_POINT ( 'NONE',  ( 0.000000000000000000, 0.000000000000000000, 0.000000000000000000 ) ) ;
#12309 = DIRECTION ( 'NONE',  ( 0.5000000000000069944, -7.511572993685774449E-15, -0.8660254037844347108 ) ) ;
#12310 = DIRECTION ( 'NONE',  ( -0.5984233124757303290, -0.8011800915434521553, 0.000000000000000000 ) ) ;
#12311 = DIRECTION ( 'NONE',  ( -0.6421085279136220514, -0.7666137478421591878, -1.662328581735448824E-15 ) ) ;
#12312 = ORIENTED_EDGE ( 'NONE', *, *, #3284, .T. ) ;
#12313 = DIRECTION ( 'NONE',  ( 0.5000000000000005551, 0.000000000000000000, -0.8660254037844384856 ) ) ;
#12314 = CARTESIAN_POINT ( 'NONE',  ( 0.000000000000000000, 1.377952755905512028, 0.000000000000000000 ) ) ;
#12315 = CARTESIAN_POINT ( 'NONE',  ( -0.05916619364927751951, -0.1856756262235988719, 0.05712045715993030459 ) ) ;
#12316 = PRODUCT_DEFINITION_SHAPE ( 'NONE', 'NONE',  #15475 ) ;
#12317 = DIRECTION ( 'NONE',  ( 0.000000000000000000, 0.000000000000000000, -1.000000000000000000 ) ) ;
#12318 = ORIENTED_EDGE ( 'NONE', *, *, #7923, .T. ) ;
#12319 = ADVANCED_FACE ( 'NONE', ( #12076 ), #14441, .F. ) ;
#12320 = VERTEX_POINT ( 'NONE', #1340 ) ;
#12321 = DIRECTION ( 'NONE',  ( -0.000000000000000000, -1.000000000000000000, -0.000000000000000000 ) ) ;
#12322 = EDGE_CURVE ( 'NONE', #6217, #15216, #2863, .T. ) ;
#12323 = EDGE_CURVE ( 'NONE', #11649, #13020, #1381, .T. ) ;
#12324 = CARTESIAN_POINT ( 'NONE',  ( -0.07874015748031501505, 0.1442356988431299225, -0.05905511811023622659 ) ) ;
#12325 = FACE_OUTER_BOUND ( 'NONE', #4150, .T. ) ;
#12326 =( CONVERSION_BASED_UNIT ( 'INCH', #213 ) LENGTH_UNIT ( ) NAMED_UNIT ( #3471 ) );
#12327 = DIRECTION ( 'NONE',  ( 0.000000000000000000, 1.000000000000000000, 0.000000000000000000 ) ) ;
#12328 = CARTESIAN_POINT ( 'NONE',  ( -0.7455328141524873997, 1.190944881889763884, 0.3622425942647021779 ) ) ;
#12329 = CARTESIAN_POINT ( 'NONE',  ( 0.06692913385832206796, -0.4881889763779528324, 9.675294977568793108E-18 ) ) ;
#12330 = FACE_OUTER_BOUND ( 'NONE', #4001, .T. ) ;
#12331 = ORIENTED_EDGE ( 'NONE', *, *, #4194, .T. ) ;
#12332 = VERTEX_POINT ( 'NONE', #12165 ) ;
#12334 = ORIENTED_EDGE ( 'NONE', *, *, #2878, .F. ) ;
#12333 = AXIS2_PLACEMENT_3D ( 'NONE', #2283, #7142, #1205 ) ;
#12335 = AXIS2_PLACEMENT_3D ( 'NONE', #5514, #7646, #11249 ) ;
#12336 = ORIENTED_EDGE ( 'NONE', *, *, #15218, .T. ) ;
#12337 = AXIS2_PLACEMENT_3D ( 'NONE', #4917, #3812, #7330 ) ;
#12338 = AXIS2_PLACEMENT_3D ( 'NONE', #4581, #5380, #13536 ) ;
#12339 = DIRECTION ( 'NONE',  ( -0.8660254037844362651, 0.000000000000000000, 0.5000000000000041078 ) ) ;
#12340 = CARTESIAN_POINT ( 'NONE',  ( -1.948352921524023396, -2.924828074509654208, 0.06159255423288990949 ) ) ;
#12341 = DIRECTION ( 'NONE',  ( -0.8660254037844395958, 0.000000000000000000, 0.4999999999999982236 ) ) ;
#12342 = CARTESIAN_POINT ( 'NONE',  ( -2.003334911435759480, -2.780488847103764982, -0.1775198577236423436 ) ) ;
#12343 = CARTESIAN_POINT ( 'NONE',  ( 1.181102362204724310, -0.1279527559055113062, 0.02559055118110236185 ) ) ;
#12344 = VECTOR ( 'NONE', #11076, 39.37007874015748143 ) ;
#12345 = VECTOR ( 'NONE', #7011, 39.37007874015748143 ) ;
#12346 = CARTESIAN_POINT ( 'NONE',  ( 0.1062992125984795477, -0.1023622047244094474, -0.2482618547481154625 ) ) ;
#12347 = AXIS2_PLACEMENT_3D ( 'NONE', #11287, #1299, #559 ) ;
#12348 = CARTESIAN_POINT ( 'NONE',  ( 0.4828087445803718181, 1.042547362667152422, 0.3474236500605413780 ) ) ;
#12349 = DIRECTION ( 'NONE',  ( 2.593979029498040879E-15, 1.000000000000000000, 2.431855340154413200E-16 ) ) ;
#12350 = AXIS2_PLACEMENT_3D ( 'NONE', #2055, #4491, #9274 ) ;
#12351 = ORIENTED_EDGE ( 'NONE', *, *, #3769, .T. ) ;
#12352 = ORIENTED_EDGE ( 'NONE', *, *, #3561, .F. ) ;
#12353 = VERTEX_POINT ( 'NONE', #8710 ) ;
#12354 = ORIENTED_EDGE ( 'NONE', *, *, #5282, .F. ) ;
#12355 = ORIENTED_EDGE ( 'NONE', *, *, #14388, .T. ) ;
#12356 = AXIS2_PLACEMENT_3D ( 'NONE', #5721, #3306, #15143 ) ;
#12357 = CARTESIAN_POINT ( 'NONE',  ( -1.419615703680148000, -0.01226548409420240640, -0.07874015748031495954 ) ) ;
#12358 = ADVANCED_FACE ( 'NONE', ( #3774 ), #8479, .F. ) ;
#12359 = AXIS2_PLACEMENT_3D ( 'NONE', #14766, #10999, #281 ) ;
#12360 = TOROIDAL_SURFACE ( 'NONE', #11873, 0.04330708661417328326, 0.003937007874015747977 ) ;
#12361 = DIRECTION ( 'NONE',  ( 0.000000000000000000, 1.000000000000000000, 0.000000000000000000 ) ) ;
#12362 = CIRCLE ( 'NONE', #10122, 0.04330708661417324162 ) ;
#12363 = B_SPLINE_CURVE_WITH_KNOTS ( 'NONE', 3,
 ( #6728, #4295, #5400, #14980 ),
 .UNSPECIFIED., .F., .F.,
 ( 4, 4 ),
 ( 0.000000000000000000, 0.0001112824830758690162 ),
 .UNSPECIFIED. ) ;
#12364 = EDGE_CURVE ( 'NONE', #14723, #9040, #12640, .T. ) ;
#12365 = EDGE_CURVE ( 'NONE', #9820, #11513, #6221, .T. ) ;
#12366 = CARTESIAN_POINT ( 'NONE',  ( 0.5452492930724234244, 1.338582677165354395, 0.2466088494548705212 ) ) ;
#12367 = CARTESIAN_POINT ( 'NONE',  ( 0.000000000000000000, 0.3622047244094487306, 0.000000000000000000 ) ) ;
#12368 = DIRECTION ( 'NONE',  ( -1.000000000000000000, 0.000000000000000000, 0.000000000000000000 ) ) ;
#12369 = DIRECTION ( 'NONE',  ( -0.000000000000000000, 0.000000000000000000, 1.000000000000000000 ) ) ;
#12370 = CARTESIAN_POINT ( 'NONE',  ( -1.900614262648875785, -2.941986504649573675, 0.05143564777245772379 ) ) ;
#12371 = VERTEX_POINT ( 'NONE', #10978 ) ;
#12372 = DIRECTION ( 'NONE',  ( 1.224646799147353207E-16, 1.000000000000000000, -0.000000000000000000 ) ) ;
#12373 = ADVANCED_FACE ( 'NONE', ( #2515 ), #5357, .T. ) ;
#12374 = AXIS2_PLACEMENT_3D ( 'NONE', #9724, #1550, #7665 ) ;
#12375 = AXIS2_PLACEMENT_3D ( 'NONE', #8761, #4214, #1548 ) ;
#12376 = AXIS2_PLACEMENT_3D ( 'NONE', #6213, #13437, #4895 ) ;
#12377 = CARTESIAN_POINT ( 'NONE',  ( -1.419615703680148000, -0.01226548409420231273, -0.07874015748031495954 ) ) ;
#12378 = CLOSED_SHELL ( 'NONE', ( #12304, #4477, #2221, #8219, #1036, #4828, #508, #670, #5363, #12577, #7144, #3575, #12358, #10102, #7697, #14732, #9731, #4721, #1900, #9713, #9405, #1780, #14157, #12319, #12136, #7393, #10959, #11733, #15200, #10642, #7221, #6970, #1963, #3501, #14324, #12031, #12471, #7613, #9051, #5871, #7855, #9068, #4809, #13003, #14861, #1465, #1842, #5702, #13658, #4432, #14515, #7481, #5900, #12966, #13045, #472, #1092, #1897, #732, #6793, #2133, #11739, #14311, #6218, #2695, #5918, #13864, #57, #3879, #1982, #3020, #7445, #330, #6246, #2833, #10061, #11234, #7680, #6937, #11960, #10550, #6030, #6037, #5838, #3839, #11050, #6079, #3613, #9804, #13438 ) ) ;
#12379 = ORIENTED_EDGE ( 'NONE', *, *, #14303, .F. ) ;
#12380 = CIRCLE ( 'NONE', #12625, 0.1476377952755906220 ) ;
#12381 = ORIENTED_EDGE ( 'NONE', *, *, #10527, .T. ) ;
#12382 = VERTEX_POINT ( 'NONE', #3841 ) ;
#12383 = EDGE_CURVE ( 'NONE', #5753, #14387, #10636, .T. ) ;
#12384 = AXIS2_PLACEMENT_3D ( 'NONE', #2051, #6821, #10447 ) ;
#12385 = VECTOR ( 'NONE', #5656, 39.37007874015748143 ) ;
#12386 = EDGE_CURVE ( 'NONE', #15216, #986, #11041, .T. ) ;
#12387 = FACE_OUTER_BOUND ( 'NONE', #889, .T. ) ;
#12388 = FACE_OUTER_BOUND ( 'NONE', #3605, .T. ) ;
#12389 = CARTESIAN_POINT ( 'NONE',  ( -0.09061599198715356018, 0.06736074103232447818, -0.007444810018878696839 ) ) ;
#12390 = CARTESIAN_POINT ( 'NONE',  ( -0.5418660417173573052, -0.4881889763779528324, 0.2355633981508970798 ) ) ;
#12391 = AXIS2_PLACEMENT_3D ( 'NONE', #1869, #6629, #11427 ) ;
#12392 = CARTESIAN_POINT ( 'NONE',  ( -0.07874015748031543138, -0.1682792322177920907, -0.05905511811023622659 ) ) ;
#12393 = ORIENTED_EDGE ( 'NONE', *, *, #4733, .F. ) ;
#12394 = CARTESIAN_POINT ( 'NONE',  ( -2.090051324975654268, -2.008999527832921572, 0.09061016354475488754 ) ) ;
#12395 = EDGE_CURVE ( 'NONE', #10993, #10478, #7879, .T. ) ;
#12396 = EDGE_CURVE ( 'NONE', #11793, #12712, #10376, .T. ) ;
#12397 = DIRECTION ( 'NONE',  ( 0.000000000000000000, 1.000000000000000000, 2.208809394877300528E-16 ) ) ;
#12398 = LINE ( 'NONE', #1742, #12716 ) ;
#12399 = CARTESIAN_POINT ( 'NONE',  ( -1.580080891953811628, 0.1020406297922293593, 0.08366141732283462196 ) ) ;
#12400 = DIRECTION ( 'NONE',  ( -0.000000000000000000, 1.000000000000000000, -0.000000000000000000 ) ) ;
#12401 = AXIS2_PLACEMENT_3D ( 'NONE', #11520, #1029, #1893 ) ;
#12402 = AXIS2_PLACEMENT_3D ( 'NONE', #2417, #10791, #71 ) ;
#12403 = VECTOR ( 'NONE', #9433, 39.37007874015748143 ) ;
#12404 = ORIENTED_EDGE ( 'NONE', *, *, #11347, .F. ) ;
#12405 = ORIENTED_EDGE ( 'NONE', *, *, #7518, .T. ) ;
#12406 = AXIS2_PLACEMENT_3D ( 'NONE', #1372, #1456, #14376 ) ;
#12407 = DIRECTION ( 'NONE',  ( 0.000000000000000000, 0.000000000000000000, -1.000000000000000000 ) ) ;
#12408 = FACE_BOUND ( 'NONE', #10532, .T. ) ;
#12409 = EDGE_CURVE ( 'NONE', #2631, #11019, #5608, .T. ) ;
#12410 = CARTESIAN_POINT ( 'NONE',  ( -2.096278492746562971, -1.821809766472917369, 0.08366141731681048244 ) ) ;
#12411 = CARTESIAN_POINT ( 'NONE',  ( 0.5860051159906326523, -0.09448818897637796532, 0.1591122789105293700 ) ) ;
#12412 = TOROIDAL_SURFACE ( 'NONE', #7651, 0.04330708661417329020, 0.003937007874015747977 ) ;
#12413 = CARTESIAN_POINT ( 'NONE',  ( -0.3441669734936866343, 2.010494531933507467, -0.03937007874015747977 ) ) ;
#12414 = CIRCLE ( 'NONE', #11401, 0.5511811023622046335 ) ;
#12415 = CARTESIAN_POINT ( 'NONE',  ( 1.928577636452524610E-17, 0.003937007874015860734, 0.1574803149606299191 ) ) ;
#12416 = CIRCLE ( 'NONE', #11668, 0.003937007874015750579 ) ;
#12417 = CARTESIAN_POINT ( 'NONE',  ( -0.4307978335858689278, -0.09448818897637796532, 0.4279391777402706820 ) ) ;
#12418 = ADVANCED_FACE ( 'NONE', ( #412 ), #8401, .F. ) ;
#12419 = EDGE_CURVE ( 'NONE', #1083, #4570, #11635, .T. ) ;
#12420 = DIRECTION ( 'NONE',  ( 0.000000000000000000, 0.000000000000000000, 1.000000000000000000 ) ) ;
#12421 = AXIS2_PLACEMENT_3D ( 'NONE', #5256, #1756, #11298 ) ;
#12422 = CARTESIAN_POINT ( 'NONE',  ( 0.1586168312385622392, -0.003937007874015747977, -0.5890199605878065903 ) ) ;
#12423 = EDGE_LOOP ( 'NONE', ( #12135, #4605, #10044, #6489 ) ) ;
#12424 = ORIENTED_EDGE ( 'NONE', *, *, #7823, .T. ) ;
#12425 = EDGE_CURVE ( 'NONE', #10501, #2195, #14141, .T. ) ;
#12426 = LINE ( 'NONE', #14705, #3372 ) ;
#12427 = ORIENTED_EDGE ( 'NONE', *, *, #11656, .T. ) ;
#12428 = AXIS2_PLACEMENT_3D ( 'NONE', #746, #5503, #13572 ) ;
#12429 = VERTEX_POINT ( 'NONE', #6649 ) ;
#12430 = AXIS2_PLACEMENT_3D ( 'NONE', #869, #4625, #3144 ) ;
#12431 = CARTESIAN_POINT ( 'NONE',  ( 0.000000000000000000, 0.5433070866141731514, 0.000000000000000000 ) ) ;
#12432 = CARTESIAN_POINT ( 'NONE',  ( -1.925142990015122679, -2.949151230150205194, 0.01280935300854439338 ) ) ;
#12433 = DIRECTION ( 'NONE',  ( 0.4999999999999998335, -0.000000000000000000, 0.8660254037844388186 ) ) ;
#12434 = DIRECTION ( 'NONE',  ( -0.000000000000000000, 0.000000000000000000, 1.000000000000000000 ) ) ;
#12435 = CARTESIAN_POINT ( 'NONE',  ( -0.6864776960422505070, 1.043307086614173151, 0.4645290592786119332 ) ) ;
#12436 = FACE_OUTER_BOUND ( 'NONE', #7560, .T. ) ;
#12437 = CARTESIAN_POINT ( 'NONE',  ( 0.05905511811023622659, 1.338626482899105241, -0.5946706712680680518 ) ) ;
#12438 = CARTESIAN_POINT ( 'NONE',  ( -0.1023622047242991467, -0.1023622047244094474, -0.5909884645248154600 ) ) ;
#12439 = CARTESIAN_POINT ( 'NONE',  ( -0.5905511811023621549, 0.3149606299212598381, 0.000000000000000000 ) ) ;
#12440 = VECTOR ( 'NONE', #3125, 39.37007874015748143 ) ;
#12441 = ORIENTED_EDGE ( 'NONE', *, *, #15054, .T. ) ;
#12442 = ADVANCED_FACE ( 'NONE', ( #9087 ), #14903, .T. ) ;
#12443 = VERTEX_POINT ( 'NONE', #11518 ) ;
#12444 = AXIS2_PLACEMENT_3D ( 'NONE', #15227, #5333, #8973 ) ;
#12445 = ORIENTED_EDGE ( 'NONE', *, *, #7132, .T. ) ;
#12446 = ORIENTED_EDGE ( 'NONE', *, *, #12469, .T. ) ;
#12447 = VECTOR ( 'NONE', #7344, 39.37007874015748854 ) ;
#12448 = ORIENTED_EDGE ( 'NONE', *, *, #15091, .F. ) ;
#12449 = AXIS2_PLACEMENT_3D ( 'NONE', #8281, #13056, #14312 ) ;
#12450 = DIRECTION ( 'NONE',  ( 1.000000000000000000, 0.000000000000000000, -1.224646799147353207E-16 ) ) ;
#12451 = DIRECTION ( 'NONE',  ( -1.000000000000000000, 0.000000000000000000, 0.000000000000000000 ) ) ;
#12452 = DIRECTION ( 'NONE',  ( 0.000000000000000000, 0.000000000000000000, -1.000000000000000000 ) ) ;
#12453 = CIRCLE ( 'NONE', #4191, 0.003937007874015724558 ) ;
#12454 = LINE ( 'NONE', #1638, #14702 ) ;
#12455 = DIRECTION ( 'NONE',  ( -0.000000000000000000, 1.000000000000000000, -0.000000000000000000 ) ) ;
#12456 = DIRECTION ( 'NONE',  ( 0.000000000000000000, 0.000000000000000000, 1.000000000000000000 ) ) ;
#12457 = AXIS2_PLACEMENT_3D ( 'NONE', #14331, #6798, #14262 ) ;
#12458 = DIRECTION ( 'NONE',  ( 0.000000000000000000, 1.000000000000000000, 0.000000000000000000 ) ) ;
#12459 = DIRECTION ( 'NONE',  ( 0.4999999999999998335, -0.000000000000000000, 0.8660254037844388186 ) ) ;
#12460 = CARTESIAN_POINT ( 'NONE',  ( -1.905882447707811345, -2.927389732709596792, -0.08665040272426297041 ) ) ;
#12461 = VERTEX_POINT ( 'NONE', #10194 ) ;
#12462 = DIRECTION ( 'NONE',  ( 0.000000000000000000, -1.000000000000000000, 0.000000000000000000 ) ) ;
#12463 = CARTESIAN_POINT ( 'NONE',  ( 0.4552518684890383138, -0.1023622047244094474, 0.3855835468379170128 ) ) ;
#12464 = AXIS2_PLACEMENT_3D ( 'NONE', #8811, #12433, #3096 ) ;
#12465 = CARTESIAN_POINT ( 'NONE',  ( -1.293236445124221312, 0.1355266887446167634, 0.05905511811023622659 ) ) ;
#12466 = ORIENTED_EDGE ( 'NONE', *, *, #4833, .T. ) ;
#12467 = ORIENTED_EDGE ( 'NONE', *, *, #1889, .T. ) ;
#12468 = AXIS2_PLACEMENT_3D ( 'NONE', #9419, #14192, #5635 ) ;
#12469 = EDGE_CURVE ( 'NONE', #6177, #11006, #7367, .T. ) ;
#12470 = ORIENTED_EDGE ( 'NONE', *, *, #4928, .T. ) ;
#12471 = ADVANCED_FACE ( 'NONE', ( #10331 ), #12544, .T. ) ;
#12472 = CIRCLE ( 'NONE', #7210, 0.03937007874015751446 ) ;
#12473 = FACE_OUTER_BOUND ( 'NONE', #8505, .T. ) ;
#12474 = CARTESIAN_POINT ( 'NONE',  ( -0.3780663654712353994, -0.2952755905511811330, 0.1046250900831904723 ) ) ;
#12475 = DIRECTION ( 'NONE',  ( -1.000000000000000000, 0.000000000000000000, 0.000000000000000000 ) ) ;
#12476 = DIRECTION ( 'NONE',  ( -1.000000000000000000, 0.000000000000000000, 0.000000000000000000 ) ) ;
#12477 = ORIENTED_EDGE ( 'NONE', *, *, #8562, .T. ) ;
#12478 = CYLINDRICAL_SURFACE ( 'NONE', #5825, 0.01968503937007875723 ) ;
#12479 = DIRECTION ( 'NONE',  ( 0.4999999999999998335, 0.000000000000000000, 0.8660254037844388186 ) ) ;
#12480 = CARTESIAN_POINT ( 'NONE',  ( 0.09842519685044813504, -0.2952755905511811330, -0.3757906139821208247 ) ) ;
#12481 = CARTESIAN_POINT ( 'NONE',  ( -1.417802900492933782, -0.04287136159519127493, 0.07363999040138466401 ) ) ;
#12482 = LENGTH_MEASURE_WITH_UNIT ( LENGTH_MEASURE( 0.02539999999999999897 ), #2920 );
#12483 = EDGE_CURVE ( 'NONE', #3171, #10010, #9388, .T. ) ;
#12484 = EDGE_CURVE ( 'NONE', #11857, #9358, #1880, .T. ) ;
#12485 = VERTEX_POINT ( 'NONE', #1969 ) ;
#12486 = EDGE_LOOP ( 'NONE', ( #8983, #5679, #6596, #6122 ) ) ;
#12487 = ORIENTED_EDGE ( 'NONE', *, *, #4452, .F. ) ;
#12488 = EDGE_CURVE ( 'NONE', #11529, #11032, #372, .T. ) ;
#12489 = CARTESIAN_POINT ( 'NONE',  ( 0.000000000000000000, 0.000000000000000000, 0.000000000000000000 ) ) ;
#12490 = DIRECTION ( 'NONE',  ( 0.5000000000000041078, 0.000000000000000000, 0.8660254037844362651 ) ) ;
#12491 = CARTESIAN_POINT ( 'NONE',  ( -2.077827123841874624, -2.289966559474202690, 0.1278948828575666996 ) ) ;
#12492 = DIRECTION ( 'NONE',  ( 0.4999999999999979461, 0.000000000000000000, 0.8660254037844398178 ) ) ;
#12493 = PRODUCT_CONTEXT ( 'NONE', #3292, 'mechanical' ) ;
#12494 = FACE_OUTER_BOUND ( 'NONE', #4169, .T. ) ;
#12495 = DIRECTION ( 'NONE',  ( 0.000000000000000000, 1.000000000000000000, 0.000000000000000000 ) ) ;
#12496 = DIRECTION ( 'NONE',  ( -0.000000000000000000, -1.000000000000000000, -0.000000000000000000 ) ) ;
#12497 = CARTESIAN_POINT ( 'NONE',  ( -1.181102362204724310, -0.1240157480314959815, -0.02559055118110236185 ) ) ;
#12498 = DIRECTION ( 'NONE',  ( 0.000000000000000000, -1.000000000000000000, 0.000000000000000000 ) ) ;
#12499 = ADVANCED_FACE ( 'NONE', ( #2986 ), #12886, .F. ) ;
#12500 = DIRECTION ( 'NONE',  ( -0.000000000000000000, -0.000000000000000000, -1.000000000000000000 ) ) ;
#12501 = VERTEX_POINT ( 'NONE', #12474 ) ;
#12502 = ADVANCED_FACE ( 'NONE', ( #2812 ), #4628, .T. ) ;
#12503 = EDGE_LOOP ( 'NONE', ( #6664, #10669, #7814, #6231 ) ) ;
#12504 = DIRECTION ( 'NONE',  ( -0.000000000000000000, -1.000000000000000000, -0.000000000000000000 ) ) ;
#12505 = ORIENTED_EDGE ( 'NONE', *, *, #6763, .F. ) ;
#12506 = ORIENTED_EDGE ( 'NONE', *, *, #12488, .T. ) ;
#12507 = EDGE_CURVE ( 'NONE', #5799, #5070, #3419, .T. ) ;
#12508 = DIRECTION ( 'NONE',  ( 0.000000000000000000, -0.000000000000000000, -1.000000000000000000 ) ) ;
#12509 = CARTESIAN_POINT ( 'NONE',  ( -1.971195541939750218, -2.816466357294567846, 0.1716894902957993574 ) ) ;
#12510 = DIRECTION ( 'NONE',  ( -0.8660254037844363761, 0.000000000000000000, 0.5000000000000038858 ) ) ;
#12511 = ADVANCED_FACE ( 'NONE', ( #553 ), #3118, .T. ) ;
#12512 = CARTESIAN_POINT ( 'NONE',  ( -1.989671392673562522, -2.818355208888676966, -0.1526115818275636249 ) ) ;
#12513 = CARTESIAN_POINT ( 'NONE',  ( 0.4305093106511115875, -0.2952755905511811330, 0.1712715594937237185 ) ) ;
#12514 = FACE_OUTER_BOUND ( 'NONE', #13600, .T. ) ;
#12515 = DIRECTION ( 'NONE',  ( 0.000000000000000000, 0.000000000000000000, -1.000000000000000000 ) ) ;
#12516 = DIRECTION ( 'NONE',  ( 0.8660254037844387076, 0.000000000000000000, 0.5000000000000001110 ) ) ;
#12517 = CARTESIAN_POINT ( 'NONE',  ( 0.06351958502452510757, -0.4921259842519685179, -0.2357441700067326174 ) ) ;
#12518 = ORIENTED_EDGE ( 'NONE', *, *, #14794, .F. ) ;
#12519 = ORIENTED_EDGE ( 'NONE', *, *, #15172, .F. ) ;
#12520 = ORIENTED_EDGE ( 'NONE', *, *, #4615, .T. ) ;
#12521 = ORIENTED_EDGE ( 'NONE', *, *, #11056, .F. ) ;
#12522 = EDGE_CURVE ( 'NONE', #5070, #8722, #12363, .T. ) ;
#12523 = ORIENTED_EDGE ( 'NONE', *, *, #1068, .F. ) ;
#12524 = CARTESIAN_POINT ( 'NONE',  ( -1.398125690441303304, -0.003404927804347051071, -0.05905511811023622659 ) ) ;
#12525 = DIRECTION ( 'NONE',  ( 0.000000000000000000, 1.000000000000000000, 2.212657494868377674E-16 ) ) ;
#12526 = LINE ( 'NONE', #14961, #3152 ) ;
#12527 = EDGE_CURVE ( 'NONE', #13891, #8036, #1621, .T. ) ;
#12528 = CARTESIAN_POINT ( 'NONE',  ( -0.07874015748031501505, 0.1442356988431297560, 0.05905511811023622659 ) ) ;
#12529 = SPHERICAL_SURFACE ( 'NONE', #14362, 0.003937007874015747977 ) ;
#12530 = EDGE_CURVE ( 'NONE', #14935, #1514, #14386, .T. ) ;
#12531 = CYLINDRICAL_SURFACE ( 'NONE', #7383, 0.6692913385826770867 ) ;
#12532 = CYLINDRICAL_SURFACE ( 'NONE', #5162, 0.003937007874015758385 ) ;
#12533 = LINE ( 'NONE', #4761, #6877 ) ;
#12534 = ORIENTED_EDGE ( 'NONE', *, *, #7700, .T. ) ;
#12535 = DIRECTION ( 'NONE',  ( 0.000000000000000000, 1.000000000000000000, 2.212657494868377674E-16 ) ) ;
#12536 = CARTESIAN_POINT ( 'NONE',  ( -0.1259842519685039353, 2.440944881889763884, -0.03937007874015747977 ) ) ;
#12537 = EDGE_LOOP ( 'NONE', ( #1899, #1745, #15434, #2174 ) ) ;
#12538 = ORIENTED_EDGE ( 'NONE', *, *, #2126, .T. ) ;
#12539 = UNCERTAINTY_MEASURE_WITH_UNIT (LENGTH_MEASURE( 1.000000000000000082E-05 ), #2257, 'distance_accuracy_value', 'NONE');
#12540 = ORIENTED_EDGE ( 'NONE', *, *, #11312, .T. ) ;
#12541 = FACE_OUTER_BOUND ( 'NONE', #12537, .T. ) ;
#12542 = DIRECTION ( 'NONE',  ( 1.000000000000000000, 0.000000000000000000, 0.000000000000000000 ) ) ;
#12543 = PRODUCT_RELATED_PRODUCT_CATEGORY ( 'part', '', ( #8171 ) ) ;
#12544 = SPHERICAL_SURFACE ( 'NONE', #4869, 0.01968503937007873988 ) ;
#12545 = CARTESIAN_POINT ( 'NONE',  ( -0.5905511811023622659, 1.377952755905512028, 0.000000000000000000 ) ) ;
#12546 = CARTESIAN_POINT ( 'NONE',  ( 0.4330708661417309036, -0.003937007874015747977, 0.4318761856142889766 ) ) ;
#12547 = ORIENTED_EDGE ( 'NONE', *, *, #5013, .T. ) ;
#12548 = DIRECTION ( 'NONE',  ( 0.000000000000000000, 0.000000000000000000, 1.000000000000000000 ) ) ;
#12549 = CARTESIAN_POINT ( 'NONE',  ( -0.4854723491485721798, 1.338626482899105241, 0.3484785681409913738 ) ) ;
#12550 = DIRECTION ( 'NONE',  ( 0.8660254037844433705, 0.000000000000000000, 0.4999999999999918954 ) ) ;
#12551 = DIRECTION ( 'NONE',  ( 0.000000000000000000, 0.000000000000000000, 1.000000000000000000 ) ) ;
#12552 = VERTEX_POINT ( 'NONE', #7588 ) ;
#12553 = ORIENTED_EDGE ( 'NONE', *, *, #693, .F. ) ;
#12554 = EDGE_LOOP ( 'NONE', ( #5415, #13308, #11530, #2463 ) ) ;
#12555 = DIRECTION ( 'NONE',  ( 0.5000000000000069944, 0.000000000000000000, 0.8660254037844347108 ) ) ;
#12556 = DIRECTION ( 'NONE',  ( -0.000000000000000000, -1.000000000000000000, 0.000000000000000000 ) ) ;
#12557 = ADVANCED_FACE ( 'NONE', ( #12388 ), #12930, .F. ) ;
#12558 = CYLINDRICAL_SURFACE ( 'NONE', #3609, 0.003937007874015749712 ) ;
#12559 = DIRECTION ( 'NONE',  ( -3.614007241618347785E-16, 0.000000000000000000, 1.000000000000000000 ) ) ;
#12560 = CARTESIAN_POINT ( 'NONE',  ( -0.002500327830562892005, -0.005471572485237196845, 0.000000000000000000 ) ) ;
#12561 = EDGE_CURVE ( 'NONE', #11758, #1514, #11209, .T. ) ;
#12562 = CARTESIAN_POINT ( 'NONE',  ( 0.06692913385832206796, -0.4881889763779528324, -0.2377126739437405434 ) ) ;
#12563 = ORIENTED_EDGE ( 'NONE', *, *, #4159, .T. ) ;
#12564 = CYLINDRICAL_SURFACE ( 'NONE', #8668, 0.03937007874015759773 ) ;
#12565 = DIRECTION ( 'NONE',  ( -0.000000000000000000, -1.000000000000000000, -0.000000000000000000 ) ) ;
#12566 = CARTESIAN_POINT ( 'NONE',  ( 0.3766253205744449772, -0.2952755905511811330, 0.09924703731238518345 ) ) ;
#12567 = EDGE_CURVE ( 'NONE', #6534, #631, #5999, .T. ) ;
#12568 = CARTESIAN_POINT ( 'NONE',  ( -0.6923203342731879539, -0.2952755905511811330, -0.2821984354013215568 ) ) ;
#12569 = ORIENTED_EDGE ( 'NONE', *, *, #8008, .F. ) ;
#12570 = ORIENTED_EDGE ( 'NONE', *, *, #3524, .F. ) ;
#12571 = ORIENTED_EDGE ( 'NONE', *, *, #5306, .T. ) ;
#12572 = ORIENTED_EDGE ( 'NONE', *, *, #2426, .T. ) ;
#12573 = EDGE_CURVE ( 'NONE', #10145, #2574, #7991, .T. ) ;
#12574 = CARTESIAN_POINT ( 'NONE',  ( 0.05905511811023622659, 1.338582677165354395, -0.8267716535433070613 ) ) ;
#12575 = CARTESIAN_POINT ( 'NONE',  ( 0.09061599198715353243, 0.07874015748031495954, 0.007444810018878659542 ) ) ;
#12576 = CARTESIAN_POINT ( 'NONE',  ( 0.000000000000000000, 0.000000000000000000, 0.000000000000000000 ) ) ;
#12577 = ADVANCED_FACE ( 'NONE', ( #13007 ), #14096, .T. ) ;
#12578 = FACE_OUTER_BOUND ( 'NONE', #4590, .T. ) ;
#12579 = CARTESIAN_POINT ( 'NONE',  ( -1.980036129185591687, -2.844263444572586952, -0.1438637502453037620 ) ) ;
#12580 = CARTESIAN_POINT ( 'NONE',  ( -0.2755905511811023167, -0.02638708502139245488, 0.05905511811023622659 ) ) ;
#12581 = EDGE_CURVE ( 'NONE', #8791, #6293, #1100, .T. ) ;
#12582 = DIRECTION ( 'NONE',  ( -0.000000000000000000, 0.000000000000000000, -1.000000000000000000 ) ) ;
#12583 = CARTESIAN_POINT ( 'NONE',  ( -2.090430742248608809, -1.869089515625215192, -0.1064913232527224946 ) ) ;
#12584 = EDGE_CURVE ( 'NONE', #10309, #12947, #8151, .T. ) ;
#12585 = AXIS2_PLACEMENT_3D ( 'NONE', #9545, #7101, #3442 ) ;
#12586 = EDGE_LOOP ( 'NONE', ( #11636, #15027, #2212, #1119 ) ) ;
#12587 = CIRCLE ( 'NONE', #5811, 0.5984251968503937480 ) ;
#12588 = VERTEX_POINT ( 'NONE', #11830 ) ;
#12589 = TOROIDAL_SURFACE ( 'NONE', #6070, 0.05905511811023621271, 0.01968503937007873988 ) ;
#12590 = ORIENTED_EDGE ( 'NONE', *, *, #1238, .F. ) ;
#12591 = EDGE_LOOP ( 'NONE', ( #8156, #6163, #11935, #11546 ) ) ;
#12592 = DIRECTION ( 'NONE',  ( 0.000000000000000000, 0.000000000000000000, -1.000000000000000000 ) ) ;
#12593 = DIRECTION ( 'NONE',  ( -0.4999999999999998335, 0.000000000000000000, -0.8660254037844388186 ) ) ;
#12594 = CARTESIAN_POINT ( 'NONE',  ( -1.596293587998444341, 0.1133155780026528781, 0.04477369844320258641 ) ) ;
#12595 = AXIS2_PLACEMENT_3D ( 'NONE', #14071, #1078, #3340 ) ;
#12596 = AXIS2_PLACEMENT_3D ( 'NONE', #14530, #3791, #433 ) ;
#12597 = CARTESIAN_POINT ( 'NONE',  ( 0.1552072824047652233, -0.003937007874015747977, -0.5870514566507987197 ) ) ;
#12598 = CIRCLE ( 'NONE', #3102, 0.5984251968503937480 ) ;
#12599 = CARTESIAN_POINT ( 'NONE',  ( -0.3492731901935981487, -0.2952755905511811330, 0.3198506632839545061 ) ) ;
#12600 = SPHERICAL_SURFACE ( 'NONE', #12391, 0.003937007874015747977 ) ;
#12601 = CIRCLE ( 'NONE', #1098, 0.007874015748031449116 ) ;
#12602 = CARTESIAN_POINT ( 'NONE',  ( -0.1062992125983150127, -0.4921259842519685179, -0.2482618547482104143 ) ) ;
#12603 = LINE ( 'NONE', #7668, #482 ) ;
#12604 = CARTESIAN_POINT ( 'NONE',  ( -1.912425819538432936, -2.839079622322270513, -0.1647229803796586289 ) ) ;
#12605 = ORIENTED_EDGE ( 'NONE', *, *, #7400, .T. ) ;
#12606 = LINE ( 'NONE', #13853, #10437 ) ;
#12607 = FACE_OUTER_BOUND ( 'NONE', #141, .T. ) ;
#12608 = EDGE_CURVE ( 'NONE', #288, #11417, #5867, .T. ) ;
#12609 = ORIENTED_EDGE ( 'NONE', *, *, #5801, .T. ) ;
#12610 = ORIENTED_EDGE ( 'NONE', *, *, #13802, .F. ) ;
#12611 = AXIS2_PLACEMENT_3D ( 'NONE', #4817, #3888, #9612 ) ;
#12612 = CIRCLE ( 'NONE', #11093, 0.01968503937007873988 ) ;
#12613 = CIRCLE ( 'NONE', #12114, 0.03937007874015761855 ) ;
#12614 = EDGE_CURVE ( 'NONE', #10501, #13129, #1144, .T. ) ;
#12615 = AXIS2_PLACEMENT_3D ( 'NONE', #15341, #3585, #1018 ) ;
#12616 = VERTEX_POINT ( 'NONE', #3221 ) ;
#12617 = CYLINDRICAL_SURFACE ( 'NONE', #11884, 0.6692913385826770867 ) ;
#12618 = DIRECTION ( 'NONE',  ( 0.4999999999999967804, 0.000000000000000000, -0.8660254037844405950 ) ) ;
#12619 = AXIS2_PLACEMENT_3D ( 'NONE', #13847, #9155, #10313 ) ;
#12620 = DIRECTION ( 'NONE',  ( -0.8660254037844347108, 0.000000000000000000, -0.5000000000000069944 ) ) ;
#12621 = AXIS2_PLACEMENT_3D ( 'NONE', #2393, #7249, #8503 ) ;
#12622 = CARTESIAN_POINT ( 'NONE',  ( -1.182291936363664364, 0.3416838286736338937, -0.04963174987406846622 ) ) ;
#12623 = VERTEX_POINT ( 'NONE', #4774 ) ;
#12624 = DIRECTION ( 'NONE',  ( 0.000000000000000000, -1.000000000000000000, 0.000000000000000000 ) ) ;
#12625 = AXIS2_PLACEMENT_3D ( 'NONE', #325, #5079, #13547 ) ;
#12626 = CIRCLE ( 'NONE', #5848, 0.01968503937007880233 ) ;
#12627 = AXIS2_PLACEMENT_3D ( 'NONE', #9193, #5252, #10049 ) ;
#12628 = DIRECTION ( 'NONE',  ( 0.000000000000000000, -1.734723475976806463E-14, -1.000000000000000000 ) ) ;
#12629 = CARTESIAN_POINT ( 'NONE',  ( -0.2755905511811023167, -0.02638708502139245488, 0.03937007874015747977 ) ) ;
#12630 = ORIENTED_EDGE ( 'NONE', *, *, #8396, .T. ) ;
#12631 = DIRECTION ( 'NONE',  ( -0.8660254037844385966, 0.000000000000000000, 0.5000000000000001110 ) ) ;
#12632 = ORIENTED_EDGE ( 'NONE', *, *, #9231, .T. ) ;
#12633 = EDGE_CURVE ( 'NONE', #11438, #731, #11887, .T. ) ;
#12635 = ORIENTED_EDGE ( 'NONE', *, *, #13737, .F. ) ;
#12634 = TOROIDAL_SURFACE ( 'NONE', #6604, 0.007874015748031495954, 0.003937007874015747977 ) ;
#12636 = AXIS2_PLACEMENT_3D ( 'NONE', #12329, #13504, #5190 ) ;
#12637 = CIRCLE ( 'NONE', #9634, 0.003937007874015721089 ) ;
#12638 = PLANE ( 'NONE',  #3416 ) ;
#12639 = CARTESIAN_POINT ( 'NONE',  ( -0.5452492930724200937, 1.043307086614173373, 0.2466088494548779875 ) ) ;
#12640 = CIRCLE ( 'NONE', #11381, 0.04330708661417324162 ) ;
#12641 = CARTESIAN_POINT ( 'NONE',  ( -0.02525249394760406899, 0.1725264476027483229, -0.03885236003516508857 ) ) ;
#12642 = CARTESIAN_POINT ( 'NONE',  ( 0.000000000000000000, 1.346456692913385877, 0.000000000000000000 ) ) ;
#12643 = DIRECTION ( 'NONE',  ( 0.000000000000000000, 0.000000000000000000, 1.000000000000000000 ) ) ;
#12644 = CARTESIAN_POINT ( 'NONE',  ( 0.01725179686542486351, 0.07136070614489377351, -0.07758808519268911574 ) ) ;
#12645 = CARTESIAN_POINT ( 'NONE',  ( -1.570515516786431975, 0.1150740656596127842, 0.05905511811023623353 ) ) ;
#12646 = ORIENTED_EDGE ( 'NONE', *, *, #8535, .F. ) ;
#12647 = CYLINDRICAL_SURFACE ( 'NONE', #5644, 0.03937007874015761855 ) ;
#12648 = CARTESIAN_POINT ( 'NONE',  ( 0.3314531923919106227, -0.2952755905511811330, 0.2641016316388982710 ) ) ;
#12649 = LINE ( 'NONE', #1919, #9887 ) ;
#12650 = AXIS2_PLACEMENT_3D ( 'NONE', #8954, #12311, #2911 ) ;
#12651 = CIRCLE ( 'NONE', #12402, 0.007874015748031449116 ) ;
#12652 = CARTESIAN_POINT ( 'NONE',  ( -0.3441669734936866343, 2.010494531933507467, 0.05905511811023622659 ) ) ;
#12653 = TOROIDAL_SURFACE ( 'NONE', #7130, 0.2303149606299203511, 0.01968503937007873988 ) ;
#12654 = ORIENTED_EDGE ( 'NONE', *, *, #14396, .F. ) ;
#12655 = DIRECTION ( 'NONE',  ( -0.8660254037844431485, 0.000000000000000000, -0.4999999999999918954 ) ) ;
#12656 = EDGE_LOOP ( 'NONE', ( #8596, #12630 ) ) ;
#12657 = EDGE_CURVE ( 'NONE', #12827, #1436, #3217, .T. ) ;
#12658 = ORIENTED_EDGE ( 'NONE', *, *, #2044, .F. ) ;
#12659 = AXIS2_PLACEMENT_3D ( 'NONE', #7551, #5275, #12278 ) ;
#12660 = VECTOR ( 'NONE', #4123, 39.37007874015748143 ) ;
#12661 = VECTOR ( 'NONE', #3754, 39.37007874015748143 ) ;
#12662 = EDGE_CURVE ( 'NONE', #3768, #2439, #7116, .T. ) ;
#12663 = DIRECTION ( 'NONE',  ( -0.5000000000000004441, 0.000000000000000000, 0.8660254037844383745 ) ) ;
#12664 = CARTESIAN_POINT ( 'NONE',  ( -1.965791048816216913, -2.881337861409273504, 0.1402741378984690979 ) ) ;
#12665 = TOROIDAL_SURFACE ( 'NONE', #9919, 0.007874015748031495954, 0.003937007874015747977 ) ;
#12666 = CARTESIAN_POINT ( 'NONE',  ( -0.5894146648244306119, -0.09448818897637796532, 0.1610807828475335490 ) ) ;
#12667 = CARTESIAN_POINT ( 'NONE',  ( -1.950690859776006425, -2.877529656554294046, -0.1430888780872220378 ) ) ;
#12668 = DIRECTION ( 'NONE',  ( -0.000000000000000000, -1.000000000000000000, -0.000000000000000000 ) ) ;
#12669 = DIRECTION ( 'NONE',  ( 0.000000000000000000, 1.000000000000000000, 0.000000000000000000 ) ) ;
#12670 = CARTESIAN_POINT ( 'NONE',  ( 0.1724006475077543565, -0.4881889763779528324, 0.1728816592724491952 ) ) ;
#12671 = CARTESIAN_POINT ( 'NONE',  ( -2.080790309745595756, -2.104291597191282115, -0.1157681807899624687 ) ) ;
#12672 = AXIS2_PLACEMENT_3D ( 'NONE', #1300, #2706, #14385 ) ;
#12673 = VERTEX_POINT ( 'NONE', #12062 ) ;
#12674 = ORIENTED_EDGE ( 'NONE', *, *, #12530, .T. ) ;
#12675 = EDGE_CURVE ( 'NONE', #749, #9606, #5243, .T. ) ;
#12676 = ORIENTED_EDGE ( 'NONE', *, *, #14681, .T. ) ;
#12677 = CIRCLE ( 'NONE', #12177, 0.007874015748031482076 ) ;
#12678 = EDGE_CURVE ( 'NONE', #13903, #13305, #1324, .T. ) ;
#12679 = EDGE_LOOP ( 'NONE', ( #9522, #10257, #8685, #11807 ) ) ;
#12680 = EDGE_CURVE ( 'NONE', #3640, #2230, #4931, .T. ) ;
#12681 = CARTESIAN_POINT ( 'NONE',  ( 8.678599364036360127E-17, 0.3228346456692913757, 0.7086614173228346081 ) ) ;
#12682 = DIRECTION ( 'NONE',  ( 0.000000000000000000, -1.000000000000000000, -0.000000000000000000 ) ) ;
#12683 = CARTESIAN_POINT ( 'NONE',  ( -2.068647409231312295, -2.591269129772357349, 0.1345927733208676091 ) ) ;
#12684 = CARTESIAN_POINT ( 'NONE',  ( 0.2393297813660762996, -0.4881889763779528324, 0.06089400679746261730 ) ) ;
#12685 = DIRECTION ( 'NONE',  ( 1.000000000000000000, -0.000000000000000000, 1.224646799147353207E-16 ) ) ;
#12686 = CARTESIAN_POINT ( 'NONE',  ( 0.000000000000000000, 0.3543307086614172485, 0.000000000000000000 ) ) ;
#12687 = AXIS2_PLACEMENT_3D ( 'NONE', #15048, #4299, #11688 ) ;
#12688 = DIRECTION ( 'NONE',  ( -0.5000000000000008882, 0.000000000000000000, 0.8660254037844381525 ) ) ;
#12689 = VERTEX_POINT ( 'NONE', #12000 ) ;
#12690 = DIRECTION ( 'NONE',  ( -0.5293839892290541638, 0.8483823383050430600, 0.000000000000000000 ) ) ;
#12691 = FACE_OUTER_BOUND ( 'NONE', #560, .T. ) ;
#12692 = VECTOR ( 'NONE', #4568, 39.37007874015748143 ) ;
#12693 = ORIENTED_EDGE ( 'NONE', *, *, #8039, .T. ) ;
#12694 = ORIENTED_EDGE ( 'NONE', *, *, #12182, .T. ) ;
#12695 = CIRCLE ( 'NONE', #5201, 0.5984251968503937480 ) ;
#12696 = VECTOR ( 'NONE', #5638, 39.37007874015748143 ) ;
#12697 = ADVANCED_FACE ( 'NONE', ( #8606 ), #1158, .T. ) ;
#12698 = PRODUCT_DEFINITION_CONTEXT ( 'detailed design', #9207, 'design' ) ;
#12699 = ORIENTED_EDGE ( 'NONE', *, *, #447, .T. ) ;
#12700 = AXIS2_PLACEMENT_3D ( 'NONE', #14969, #6961, #9076 ) ;
#12701 = CARTESIAN_POINT ( 'NONE',  ( -0.3669897256266691499, -0.2952755905511811330, 0.2891647237797815850 ) ) ;
#12702 = EDGE_CURVE ( 'NONE', #15414, #925, #5373, .T. ) ;
#12703 = CIRCLE ( 'NONE', #14463, 0.007874015748031516770 ) ;
#12704 = DIRECTION ( 'NONE',  ( 0.000000000000000000, -1.000000000000000000, 0.000000000000000000 ) ) ;
#12705 = SHAPE_REPRESENTATION ( 'Spider', ( #11481 ), #5701 ) ;
#12706 = CARTESIAN_POINT ( 'NONE',  ( -0.4861941749621833675, 1.043307086614173373, 0.3488953144687877983 ) ) ;
#12707 = CARTESIAN_POINT ( 'NONE',  ( 0.000000000000000000, 0.3070866141732283561, 0.5984251968503937480 ) ) ;
#12709 = AXIS2_PLACEMENT_3D ( 'NONE', #2167, #7291, #11734 ) ;
#12708 = CARTESIAN_POINT ( 'NONE',  ( -1.957251767099916107, -2.772329397582958599, 0.1771653543307079026 ) ) ;
#12710 = B_SPLINE_CURVE_WITH_KNOTS ( 'NONE', 3,
 ( #10005, #12215, #14785, #4039, #1706, #13590 ),
 .UNSPECIFIED., .F., .F.,
 ( 4, 2, 4 ),
 ( 0.000000000000000000, 0.0003645138504237786640, 0.0007290277008475573280 ),
 .UNSPECIFIED. ) ;
#12711 = CARTESIAN_POINT ( 'NONE',  ( 0.06692913385832208184, -0.2952755905511811330, -0.4190977005962941426 ) ) ;
#12712 = VERTEX_POINT ( 'NONE', #10798 ) ;
#12713 = DIRECTION ( 'NONE',  ( -1.000000000000000000, -0.000000000000000000, 0.000000000000000000 ) ) ;
#12714 = ADVANCED_FACE ( 'NONE', ( #8526 ), #12292, .F. ) ;
#12715 = CARTESIAN_POINT ( 'NONE',  ( 7.328595018519593763E-17, 1.370078740157480546, -0.5984251968503937480 ) ) ;
#12716 = VECTOR ( 'NONE', #10203, 39.37007874015748143 ) ;
#12717 = CARTESIAN_POINT ( 'NONE',  ( -1.396183715708124051, -0.02562187435717607278, -0.04038159613861123237 ) ) ;
#12718 = CARTESIAN_POINT ( 'NONE',  ( -1.187897378299091367, 0.3305578035811536641, 0.05905511811023621271 ) ) ;
#12719 = ORIENTED_EDGE ( 'NONE', *, *, #10576, .F. ) ;
#12720 = DIRECTION ( 'NONE',  ( -0.000000000000000000, 0.000000000000000000, 1.000000000000000000 ) ) ;
#12721 = ORIENTED_EDGE ( 'NONE', *, *, #1388, .T. ) ;
#12722 = ORIENTED_EDGE ( 'NONE', *, *, #4351, .F. ) ;
#12723 = VECTOR ( 'NONE', #9890, 39.37007874015748143 ) ;
#12724 = ORIENTED_EDGE ( 'NONE', *, *, #4229, .F. ) ;
#12725 = CARTESIAN_POINT ( 'NONE',  ( 0.000000000000000000, 0.4133858267716535306, 0.000000000000000000 ) ) ;
#12726 = CARTESIAN_POINT ( 'NONE',  ( 0.000000000000000000, 0.07874015748031495954, 0.000000000000000000 ) ) ;
#12727 = AXIS2_PLACEMENT_3D ( 'NONE', #8532, #2666, #2573 ) ;
#12728 = LINE ( 'NONE', #10283, #15376 ) ;
#12729 = CARTESIAN_POINT ( 'NONE',  ( -0.4572203724260467950, -0.4881889763779528324, 0.3821739980041202744 ) ) ;
#12730 = DIRECTION ( 'NONE',  ( 0.000000000000000000, 1.000000000000000000, 0.000000000000000000 ) ) ;
#12731 = DIRECTION ( 'NONE',  ( 3.942553354492736135E-16, 0.000000000000000000, -1.000000000000000000 ) ) ;
#12732 = ORIENTED_EDGE ( 'NONE', *, *, #13418, .F. ) ;
#12733 = FACE_OUTER_BOUND ( 'NONE', #6789, .T. ) ;
#12734 = EDGE_CURVE ( 'NONE', #11619, #4513, #6121, .T. ) ;
#12735 = CARTESIAN_POINT ( 'NONE',  ( 0.9851651268172137987, -1.725292181286280480, -0.08366141732283417787 ) ) ;
#12736 = VECTOR ( 'NONE', #15189, 39.37007874015748143 ) ;
#12737 = CYLINDRICAL_SURFACE ( 'NONE', #14181, 0.003937007874015724558 ) ;
#12738 = AXIS2_PLACEMENT_3D ( 'NONE', #11010, #7486, #9614 ) ;
#12739 = EDGE_LOOP ( 'NONE', ( #7952, #14085, #4777, #10492 ) ) ;
#12740 = DIRECTION ( 'NONE',  ( 0.8660254037844433705, 0.000000000000000000, 0.4999999999999918954 ) ) ;
#12741 = ORIENTED_EDGE ( 'NONE', *, *, #6298, .T. ) ;
#12742 = EDGE_LOOP ( 'NONE', ( #14033, #6790, #7732, #7140 ) ) ;
#12743 = DIRECTION ( 'NONE',  ( -1.349229370204184172E-15, -1.000000000000000000, 0.000000000000000000 ) ) ;
#12744 = CARTESIAN_POINT ( 'NONE',  ( 0.000000000000000000, 0.003937007874015860734, 0.000000000000000000 ) ) ;
#12745 = CARTESIAN_POINT ( 'NONE',  ( -0.05314960629921194196, -0.09842519685039370636, 0.09205781851251791659 ) ) ;
#12746 = CARTESIAN_POINT ( 'NONE',  ( -1.276200637803905691, -0.1988000726501942539, -0.08366141732283455257 ) ) ;
#12747 = SPHERICAL_SURFACE ( 'NONE', #13906, 0.003937007874015747977 ) ;
#12748 = CARTESIAN_POINT ( 'NONE',  ( 0.09842519685044820443, -0.4881889763779528324, -0.5870514566507987197 ) ) ;
#12749 = CARTESIAN_POINT ( 'NONE',  ( -2.087452354246647879, -2.011709019740274940, -0.09152848164307673950 ) ) ;
#12750 = ORIENTED_EDGE ( 'NONE', *, *, #8636, .F. ) ;
#12751 = EDGE_CURVE ( 'NONE', #7178, #238, #14, .T. ) ;
#12752 = ORIENTED_EDGE ( 'NONE', *, *, #13134, .T. ) ;
#12753 = ORIENTED_EDGE ( 'NONE', *, *, #3199, .F. ) ;
#12754 = VERTEX_POINT ( 'NONE', #14422 ) ;
#12755 = DIRECTION ( 'NONE',  ( 0.000000000000000000, -1.000000000000000000, 0.000000000000000000 ) ) ;
#12756 = FACE_OUTER_BOUND ( 'NONE', #12767, .T. ) ;
#12757 = FACE_OUTER_BOUND ( 'NONE', #12804, .T. ) ;
#12758 = DIRECTION ( 'NONE',  ( 0.4999999999999966693, 0.000000000000000000, -0.8660254037844405950 ) ) ;
#12759 = CARTESIAN_POINT ( 'NONE',  ( 0.1463103599445507719, -0.09842519685039370636, -0.08447232569921737932 ) ) ;
#12760 = CARTESIAN_POINT ( 'NONE',  ( 0.1552072824047652233, -0.003937007874015747977, -0.5909884645248143498 ) ) ;
#12761 = EDGE_CURVE ( 'NONE', #6873, #11758, #14154, .T. ) ;
#12762 = ORIENTED_EDGE ( 'NONE', *, *, #4321, .T. ) ;
#12763 = CARTESIAN_POINT ( 'NONE',  ( 0.000000000000000000, 1.370078740157480546, -0.5905511811023621549 ) ) ;
#12764 = FACE_OUTER_BOUND ( 'NONE', #10221, .T. ) ;
#12765 = ORIENTED_EDGE ( 'NONE', *, *, #2264, .F. ) ;
#12766 = EDGE_CURVE ( 'NONE', #9167, #1544, #6622, .T. ) ;
#12767 = EDGE_LOOP ( 'NONE', ( #3300, #4062, #7948, #964 ) ) ;
#12768 = EDGE_LOOP ( 'NONE', ( #1713, #2509, #868, #12831 ) ) ;
#12769 = CARTESIAN_POINT ( 'NONE',  ( -0.4478092776764608374, 1.043307086614173373, 0.3267337836880595536 ) ) ;
#12770 = EDGE_CURVE ( 'NONE', #5808, #6948, #2565, .T. ) ;
#12771 = CARTESIAN_POINT ( 'NONE',  ( -1.100415514366356762, -0.04998955061627542718, -0.05905511811023622659 ) ) ;
#12772 = CARTESIAN_POINT ( 'NONE',  ( -1.938628142022554401, -2.911908481707071950, 0.1097354202932025180 ) ) ;
#12773 = DIRECTION ( 'NONE',  ( -0.8660254037844395958, 0.000000000000000000, -0.4999999999999982236 ) ) ;
#12774 = EDGE_CURVE ( 'NONE', #2263, #11243, #10961, .T. ) ;
#12775 = ORIENTED_EDGE ( 'NONE', *, *, #7746, .T. ) ;
#12776 = LINE ( 'NONE', #11593, #2175 ) ;
#12777 = DIRECTION ( 'NONE',  ( -1.000000000000000000, 0.000000000000000000, 0.000000000000000000 ) ) ;
#12778 = DIRECTION ( 'NONE',  ( 0.4999999999999966693, 0.000000000000000000, 0.8660254037844405950 ) ) ;
#12779 = DIRECTION ( 'NONE',  ( 0.5984233124757303290, 0.8011800915434521553, 0.000000000000000000 ) ) ;
#12780 = ORIENTED_EDGE ( 'NONE', *, *, #10185, .F. ) ;
#12781 = ADVANCED_FACE ( 'NONE', ( #14651 ), #13139, .F. ) ;
#12782 = CARTESIAN_POINT ( 'NONE',  ( 0.1552072824047652788, -0.003937007874015747977, -0.5870514566507987197 ) ) ;
#12783 = ADVANCED_FACE ( 'NONE', ( #3991 ), #12531, .F. ) ;
#12784 = EDGE_LOOP ( 'NONE', ( #3716, #12139, #9062, #5632 ) ) ;
#12785 = ORIENTED_EDGE ( 'NONE', *, *, #14962, .T. ) ;
#12786 = PRODUCT_DEFINITION_SHAPE ( 'NONE', 'NONE',  #15498 ) ;
#12787 = EDGE_LOOP ( 'NONE', ( #8275, #14018, #1286, #6618 ) ) ;
#12788 = DIRECTION ( 'NONE',  ( -0.000000000000000000, -1.000000000000000000, -0.000000000000000000 ) ) ;
#12789 = CARTESIAN_POINT ( 'NONE',  ( -1.181102362204724310, 0.1240157480314959815, 0.02952755905511811330 ) ) ;
#12790 = LINE ( 'NONE', #973, #15362 ) ;
#12791 = DIRECTION ( 'NONE',  ( -0.000000000000000000, 1.000000000000000000, 0.000000000000000000 ) ) ;
#12792 = ITEM_DEFINED_TRANSFORMATION ( 'NONE', 'NONE', #7602,  #11481 ) ;
#12793 = DIRECTION ( 'NONE',  ( -0.8660254037844383745, 0.000000000000000000, -0.5000000000000004441 ) ) ;
#12794 = CARTESIAN_POINT ( 'NONE',  ( 0.000000000000000000, 1.338582677165354395, 0.000000000000000000 ) ) ;
#12795 = VERTEX_POINT ( 'NONE', #7666 ) ;
#12796 = CARTESIAN_POINT ( 'NONE',  ( 0.1734555655881918346, -0.1023622047244094474, 0.1728816592724491952 ) ) ;
#12797 = CARTESIAN_POINT ( 'NONE',  ( 0.1062992125984794506, -0.09842519685039370636, 4.223515039848272764E-17 ) ) ;
#12798 = FACE_OUTER_BOUND ( 'NONE', #6295, .T. ) ;
#12799 = SURFACE_STYLE_FILL_AREA ( #11717 ) ;
#12800 = EDGE_CURVE ( 'NONE', #13296, #12353, #10388, .T. ) ;
#12801 = ORIENTED_EDGE ( 'NONE', *, *, #12323, .T. ) ;
#12802 = ORIENTED_EDGE ( 'NONE', *, *, #6776, .F. ) ;
#12803 = LINE ( 'NONE', #5422, #11180 ) ;
#12804 = EDGE_LOOP ( 'NONE', ( #2752, #8263, #6969, #11021 ) ) ;
#12805 = ORIENTED_EDGE ( 'NONE', *, *, #4353, .F. ) ;
#12806 = ADVANCED_FACE ( 'NONE', ( #15032 ), #6399, .T. ) ;
#12807 = ORIENTED_EDGE ( 'NONE', *, *, #15077, .F. ) ;
#12808 = CARTESIAN_POINT ( 'NONE',  ( 0.000000000000000000, 0.4094488188976377896, -0.03937007874015747977 ) ) ;
#12809 = DIRECTION ( 'NONE',  ( 0.000000000000000000, -1.000000000000000000, 0.000000000000000000 ) ) ;
#12810 = CARTESIAN_POINT ( 'NONE',  ( 0.000000000000000000, 2.401574803149606918, 0.5433070866141731514 ) ) ;
#12811 = CARTESIAN_POINT ( 'NONE',  ( -0.4307978335858689278, -0.09448818897637796532, 0.4279391777402706265 ) ) ;
#12812 = DIRECTION ( 'NONE',  ( 0.000000000000000000, 0.000000000000000000, -1.000000000000000000 ) ) ;
#12813 = CARTESIAN_POINT ( 'NONE',  ( -0.2362204724409448231, -0.02638708502139245488, 0.03937007874015747977 ) ) ;
#12814 = DIRECTION ( 'NONE',  ( 0.8660254037844383745, 0.000000000000000000, -0.5000000000000004441 ) ) ;
#12815 = ORIENTED_EDGE ( 'NONE', *, *, #6269, .T. ) ;
#12816 = B_SPLINE_CURVE_WITH_KNOTS ( 'NONE', 3,
 ( #2514, #13091, #13022, #7288, #10902, #190 ),
 .UNSPECIFIED., .F., .F.,
 ( 4, 2, 4 ),
 ( -2.828444569877115420E-06, 0.0001777364543001118868, 0.0003583013531701008544 ),
 .UNSPECIFIED. ) ;
#12817 = VERTEX_POINT ( 'NONE', #4137 ) ;
#12818 = VERTEX_POINT ( 'NONE', #4055 ) ;
#12819 = VERTEX_POINT ( 'NONE', #1640 ) ;
#12820 = DIRECTION ( 'NONE',  ( -3.942553354492736135E-16, 0.000000000000000000, 1.000000000000000000 ) ) ;
#12821 = CARTESIAN_POINT ( 'NONE',  ( -0.2359202325321149429, -0.1023622047244094474, 0.06286251073437545966 ) ) ;
#12822 = DIRECTION ( 'NONE',  ( 0.000000000000000000, 0.000000000000000000, -1.000000000000000000 ) ) ;
#12823 = CARTESIAN_POINT ( 'NONE',  ( 0.05905511811023622659, 1.338597318737259734, -0.5949473527966270270 ) ) ;
#12824 = CARTESIAN_POINT ( 'NONE',  ( -0.5649606299212329708, -0.09448818897637796532, 0.2034364137499347913 ) ) ;
#12825 = VECTOR ( 'NONE', #12050, 39.37007874015748143 ) ;
#12826 = CARTESIAN_POINT ( 'NONE',  ( -1.943436547385579249, -2.816558498006583644, -0.1716660038806392119 ) ) ;
#12827 = VERTEX_POINT ( 'NONE', #8764 ) ;
#12828 = DIRECTION ( 'NONE',  ( 1.000000000000000000, 0.000000000000000000, 0.000000000000000000 ) ) ;
#12829 = FACE_OUTER_BOUND ( 'NONE', #3520, .T. ) ;
#12830 = ORIENTED_EDGE ( 'NONE', *, *, #3852, .F. ) ;
#12831 = ORIENTED_EDGE ( 'NONE', *, *, #10743, .F. ) ;
#12832 = ADVANCED_FACE ( 'NONE', ( #7567 ), #1892, .T. ) ;
#12833 = ORIENTED_EDGE ( 'NONE', *, *, #7926, .T. ) ;
#12834 = AXIS2_PLACEMENT_3D ( 'NONE', #96, #14204, #15373 ) ;
#12835 = TOROIDAL_SURFACE ( 'NONE', #3834, 0.5590551181102362266, 0.007874015748031495954 ) ;
#12836 = EDGE_CURVE ( 'NONE', #1428, #13129, #644, .T. ) ;
#12837 = CARTESIAN_POINT ( 'NONE',  ( -0.09061599198715356018, 0.000000000000000000, -0.007444810018878696839 ) ) ;
#12838 = TOROIDAL_SURFACE ( 'NONE', #6067, 0.05905511811023621271, 0.01968503937007873988 ) ;
#12839 = AXIS2_PLACEMENT_3D ( 'NONE', #9645, #83, #3758 ) ;
#12840 = ADVANCED_FACE ( 'NONE', ( #11267 ), #540, .T. ) ;
#12841 = DIRECTION ( 'NONE',  ( -1.000000000000000000, 0.000000000000000000, 0.000000000000000000 ) ) ;
#12842 = CARTESIAN_POINT ( 'NONE',  ( -1.927226688427879475, -2.943474258813137290, -0.04731147916820623023 ) ) ;
#12843 = CARTESIAN_POINT ( 'NONE',  ( 0.5084014747882494856, -0.4881889763779528324, 0.2935257283254013583 ) ) ;
#12844 = FACE_OUTER_BOUND ( 'NONE', #1480, .T. ) ;
#12845 = ORIENTED_EDGE ( 'NONE', *, *, #12225, .T. ) ;
#12846 = CARTESIAN_POINT ( 'NONE',  ( -2.100501784635051550, -1.630597114118274238, -0.1033464566929129386 ) ) ;
#12847 = CARTESIAN_POINT ( 'NONE',  ( 0.1743691514447621993, -0.4881889763779528324, 0.1734091183126679481 ) ) ;
#12848 = CIRCLE ( 'NONE', #13586, 0.2362204724409449619 ) ;
#12849 = AXIS2_PLACEMENT_3D ( 'NONE', #11145, #506, #13743 ) ;
#12850 = CARTESIAN_POINT ( 'NONE',  ( -0.05905511811023622659, 1.338597318737259734, -0.5949473527966270270 ) ) ;
#12851 = DIRECTION ( 'NONE',  ( -0.000000000000000000, 0.000000000000000000, 1.000000000000000000 ) ) ;
#12852 = ORIENTED_EDGE ( 'NONE', *, *, #10855, .F. ) ;
#12853 = AXIS2_PLACEMENT_3D ( 'NONE', #3655, #12109, #7694 ) ;
#12854 = CARTESIAN_POINT ( 'NONE',  ( -1.596293587998444563, 0.1133155780026525727, 0.04477369844320282927 ) ) ;
#12855 = TOROIDAL_SURFACE ( 'NONE', #11087, 0.007874015748031495954, 0.003937007874015747977 ) ;
#12856 = EDGE_LOOP ( 'NONE', ( #7675, #12467, #5403 ) ) ;
#12857 = VERTEX_POINT ( 'NONE', #14879 ) ;
#12858 = B_SPLINE_CURVE_WITH_KNOTS ( 'NONE', 3,
 ( #13478, #5154, #2743, #10026, #11202, #7513, #12299, #12377 ),
 .UNSPECIFIED., .F., .F.,
 ( 4, 2, 2, 4 ),
 ( 0.000000000000000000, 0.0004305386933195752574, 0.0006458080399793631301, 0.0008610773866391509485 ),
 .UNSPECIFIED. ) ;
#12859 = EDGE_CURVE ( 'NONE', #8791, #1599, #11127, .T. ) ;
#12860 = EDGE_LOOP ( 'NONE', ( #4260, #12945, #10375, #15393, #8475, #11720 ) ) ;
#12861 = CARTESIAN_POINT ( 'NONE',  ( 0.000000000000000000, 0.000000000000000000, 0.08858267716535432601 ) ) ;
#12862 = CARTESIAN_POINT ( 'NONE',  ( -0.1574803149606299191, -0.09448818897637796532, -0.5870514566507987197 ) ) ;
#12863 = CIRCLE ( 'NONE', #6089, 0.03937007874015751446 ) ;
#12864 = AXIS2_PLACEMENT_3D ( 'NONE', #15244, #7953, #6841 ) ;
#12865 = EDGE_CURVE ( 'NONE', #777, #9061, #149, .T. ) ;
#12866 = LINE ( 'NONE', #6669, #11350 ) ;
#12867 = DIRECTION ( 'NONE',  ( -0.000000000000000000, -1.000000000000000000, -0.000000000000000000 ) ) ;
#12868 = CIRCLE ( 'NONE', #11096, 0.007874015748031499423 ) ;
#12869 = ITEM_DEFINED_TRANSFORMATION ( 'NONE', 'NONE', #859,  #11481 ) ;
#12870 = PLANE ( 'NONE',  #11446 ) ;
#12871 = DIRECTION ( 'NONE',  ( -0.000000000000000000, -0.000000000000000000, -1.000000000000000000 ) ) ;
#12872 = AXIS2_PLACEMENT_3D ( 'NONE', #6176, #3829, #14661 ) ;
#12873 = ORIENTED_EDGE ( 'NONE', *, *, #15077, .T. ) ;
#12874 = CARTESIAN_POINT ( 'NONE',  ( -0.1181102362204724254, 2.448818897637795367, 0.03937007874015747977 ) ) ;
#12875 = CARTESIAN_POINT ( 'NONE',  ( 0.09842519685044820443, -0.4921259842519685179, -0.5909884645248143498 ) ) ;
#12876 = SURFACE_STYLE_FILL_AREA ( #6827 ) ;
#12877 = CARTESIAN_POINT ( 'NONE',  ( 0.02952755905509091630, -0.09842519685039370636, -0.05114323250690790829 ) ) ;
#12878 = ORIENTED_EDGE ( 'NONE', *, *, #8765, .T. ) ;
#12879 = AXIS2_PLACEMENT_3D ( 'NONE', #2767, #12495, #7536 ) ;
#12880 = AXIS2_PLACEMENT_3D ( 'NONE', #7662, #13703, #9864 ) ;
#12881 = CIRCLE ( 'NONE', #11883, 0.003937007874015724558 ) ;
#12882 = TOROIDAL_SURFACE ( 'NONE', #2624, 0.04330708661417328326, 0.003937007874015747977 ) ;
#12883 = VERTEX_POINT ( 'NONE', #1790 ) ;
#12884 = LINE ( 'NONE', #14222, #8310 ) ;
#12885 = ORIENTED_EDGE ( 'NONE', *, *, #11716, .F. ) ;
#12886 = TOROIDAL_SURFACE ( 'NONE', #6610, 0.007874015748031495954, 0.003937007874015747977 ) ;
#12887 = EDGE_CURVE ( 'NONE', #6733, #1879, #2637, .T. ) ;
#12888 = ORIENTED_EDGE ( 'NONE', *, *, #252, .F. ) ;
#12889 = VERTEX_POINT ( 'NONE', #9006 ) ;
#12890 = CARTESIAN_POINT ( 'NONE',  ( -0.3706061991976995484, -0.003937007874015747977, -0.2139695888701363957 ) ) ;
#12891 = CARTESIAN_POINT ( 'NONE',  ( 0.5084014747882494856, -0.09842519685039370636, 0.2935257283254013583 ) ) ;
#12892 = CARTESIAN_POINT ( 'NONE',  ( -1.932762117030202953, -2.849396711222250023, -0.1599284002103965874 ) ) ;
#12893 = ADVANCED_FACE ( 'NONE', ( #13778 ), #12600, .T. ) ;
#12894 = AXIS2_PLACEMENT_3D ( 'NONE', #4791, #13100, #9671 ) ;
#12895 = DIRECTION ( 'NONE',  ( -0.000000000000000000, 1.000000000000000000, 0.000000000000000000 ) ) ;
#12896 = CIRCLE ( 'NONE', #4383, 0.007874015748031516770 ) ;
#12897 = CARTESIAN_POINT ( 'NONE',  ( 1.181102362204724310, 4.044111181948214319E-16, -0.02559055118110236185 ) ) ;
#12898 = CARTESIAN_POINT ( 'NONE',  ( 1.305118110236220152, 4.044111181948214319E-16, -0.02952755905511811330 ) ) ;
#12899 = CARTESIAN_POINT ( 'NONE',  ( -1.387704745771440429, -0.02010536753476148755, 0.05905511811023627516 ) ) ;
#12900 = EDGE_CURVE ( 'NONE', #14427, #776, #3043, .T. ) ;
#12901 = DIRECTION ( 'NONE',  ( -1.000000000000000000, 0.000000000000000000, 0.000000000000000000 ) ) ;
#12902 = SURFACE_SIDE_STYLE ('',( #8116 ) ) ;
#12903 = ORIENTED_EDGE ( 'NONE', *, *, #3723, .T. ) ;
#12904 = ORIENTED_EDGE ( 'NONE', *, *, #10422, .F. ) ;
#12905 = AXIS2_PLACEMENT_3D ( 'NONE', #7959, #13918, #9142 ) ;
#12906 = ORIENTED_EDGE ( 'NONE', *, *, #13234, .F. ) ;
#12907 = AXIS2_PLACEMENT_3D ( 'NONE', #2324, #3353, #11907 ) ;
#12908 = VECTOR ( 'NONE', #14828, 39.37007874015748143 ) ;
#12909 = VERTEX_POINT ( 'NONE', #2796 ) ;
#12910 = CIRCLE ( 'NONE', #7642, 0.003937007874015721089 ) ;
#12911 = FACE_OUTER_BOUND ( 'NONE', #14759, .T. ) ;
#12912 = FACE_OUTER_BOUND ( 'NONE', #14525, .T. ) ;
#12913 = CARTESIAN_POINT ( 'NONE',  ( -0.06867854503139053657, 0.1655849054964026734, 0.03830121270948940587 ) ) ;
#12914 = DIRECTION ( 'NONE',  ( 0.8660254037844385966, -0.000000000000000000, -0.5000000000000001110 ) ) ;
#12915 = CIRCLE ( 'NONE', #2159, 0.03937007874015751446 ) ;
#12916 = CIRCLE ( 'NONE', #12174, 0.1653543307086614012 ) ;
#12917 = DIRECTION ( 'NONE',  ( 1.000000000000000000, 0.000000000000000000, 0.000000000000000000 ) ) ;
#12918 = ORIENTED_EDGE ( 'NONE', *, *, #747, .F. ) ;
#12919 = CARTESIAN_POINT ( 'NONE',  ( 0.5905511811023622659, -0.2952755905511811330, -0.4584677793364514420 ) ) ;
#12920 = ADVANCED_FACE ( 'NONE', ( #10249 ), #11395, .T. ) ;
#12921 = CARTESIAN_POINT ( 'NONE',  ( 0.000000000000000000, 0.003937007874015860734, -0.1574803149606299191 ) ) ;
#12922 = TOROIDAL_SURFACE ( 'NONE', #6146, 0.007874015748031495954, 0.003937007874015747977 ) ;
#12923 = PRODUCT_DEFINITION_SHAPE ( 'NONE', 'NONE',  #15495 ) ;
#12924 = ORIENTED_EDGE ( 'NONE', *, *, #8690, .T. ) ;
#12925 = ORIENTED_EDGE ( 'NONE', *, *, #2460, .F. ) ;
#12926 = EDGE_LOOP ( 'NONE', ( #6235, #5232, #7715, #7559, #5435, #814 ) ) ;
#12927 = CIRCLE ( 'NONE', #14433, 0.003937007874015724558 ) ;
#12928 = CARTESIAN_POINT ( 'NONE',  ( -0.4307978335858689833, 0.000000000000000000, 0.4279391777402706265 ) ) ;
#12929 = FACE_OUTER_BOUND ( 'NONE', #12004, .T. ) ;
#12930 = SPHERICAL_SURFACE ( 'NONE', #3878, 0.003937007874015747977 ) ;
#12931 = LINE ( 'NONE', #5776, #4932 ) ;
#12932 = DIRECTION ( 'NONE',  ( 0.8660254037844363761, 0.000000000000000000, -0.5000000000000039968 ) ) ;
#12933 = CARTESIAN_POINT ( 'NONE',  ( -1.187809996374852739, 0.3305575196848991038, -0.05905511802097350438 ) ) ;
#12934 = EDGE_LOOP ( 'NONE', ( #14290, #10914, #4815, #1040 ) ) ;
#12935 = DIRECTION ( 'NONE',  ( 1.445602896647339903E-16, 0.000000000000000000, -1.000000000000000000 ) ) ;
#12936 = DIRECTION ( 'NONE',  ( 0.000000000000000000, 0.000000000000000000, -1.000000000000000000 ) ) ;
#12937 = CIRCLE ( 'NONE', #14947, 0.003937007874015758385 ) ;
#12938 = FACE_BOUND ( 'NONE', #2176, .T. ) ;
#12939 = CARTESIAN_POINT ( 'NONE',  ( -1.603592887480403295, 0.1030246510253539083, 0.05618170010999483377 ) ) ;
#12940 = EDGE_LOOP ( 'NONE', ( #13922, #7069, #3459, #927 ) ) ;
#12941 = LINE ( 'NONE', #10436, #12696 ) ;
#12942 = CIRCLE ( 'NONE', #2185, 0.003937007874015724558 ) ;
#12943 = ORIENTED_EDGE ( 'NONE', *, *, #6298, .F. ) ;
#12944 = EDGE_CURVE ( 'NONE', #5535, #12443, #7631, .T. ) ;
#12945 = ORIENTED_EDGE ( 'NONE', *, *, #12507, .T. ) ;
#12946 = CIRCLE ( 'NONE', #9955, 0.003937007874015758385 ) ;
#12947 = VERTEX_POINT ( 'NONE', #12824 ) ;
#12948 = ORIENTED_EDGE ( 'NONE', *, *, #5458, .F. ) ;
#12949 = CARTESIAN_POINT ( 'NONE',  ( -0.5084014747882513729, -0.4881889763779528324, 0.2935257283253980831 ) ) ;
#12950 = CYLINDRICAL_SURFACE ( 'NONE', #6133, 0.003937007874015724558 ) ;
#12951 = DIRECTION ( 'NONE',  ( -0.000000000000000000, -1.000000000000000000, -0.000000000000000000 ) ) ;
#12952 = DIRECTION ( 'NONE',  ( 0.000000000000000000, 0.000000000000000000, -1.000000000000000000 ) ) ;
#12953 = ITEM_DEFINED_TRANSFORMATION ( 'NONE', 'NONE', #1866,  #11481 ) ;
#12954 = CARTESIAN_POINT ( 'NONE',  ( 0.000000000000000000, 0.000000000000000000, 0.000000000000000000 ) ) ;
#12955 = AXIS2_PLACEMENT_3D ( 'NONE', #9443, #3485, #15387 ) ;
#12956 = PLANE ( 'NONE',  #1138 ) ;
#12957 = VERTEX_POINT ( 'NONE', #14076 ) ;
#12958 = FACE_OUTER_BOUND ( 'NONE', #6653, .T. ) ;
#12959 = CARTESIAN_POINT ( 'NONE',  ( -1.580259682938329524, 0.1018956540307723729, 0.04477369844403742555 ) ) ;
#12960 =( LENGTH_UNIT ( ) NAMED_UNIT ( * ) SI_UNIT ( $, .METRE. ) );
#12961 = EDGE_CURVE ( 'NONE', #7280, #9296, #15370, .T. ) ;
#12962 = CYLINDRICAL_SURFACE ( 'NONE', #10188, 0.003937007874015759253 ) ;
#12963 = ORIENTED_EDGE ( 'NONE', *, *, #522, .T. ) ;
#12964 = AXIS2_PLACEMENT_3D ( 'NONE', #3183, #15168, #8481 ) ;
#12965 = VERTEX_POINT ( 'NONE', #7974 ) ;
#12966 = ADVANCED_FACE ( 'NONE', ( #768 ), #15100, .T. ) ;
#12967 = CARTESIAN_POINT ( 'NONE',  ( 0.1724006475077543565, -0.4921259842519685179, 0.1768186671464649640 ) ) ;
#12968 = ORIENTED_EDGE ( 'NONE', *, *, #15282, .T. ) ;
#12969 = TOROIDAL_SURFACE ( 'NONE', #5687, 0.04527559055118110520, 0.005905511811023621965 ) ;
#12970 = ORIENTED_EDGE ( 'NONE', *, *, #2745, .T. ) ;
#12971 = VERTEX_POINT ( 'NONE', #5613 ) ;
#12972 = CARTESIAN_POINT ( 'NONE',  ( 0.3623183339751714360, -0.2952755905511811330, 0.1319014807535661138 ) ) ;
#12973 = DIRECTION ( 'NONE',  ( 0.000000000000000000, 0.000000000000000000, -1.000000000000000000 ) ) ;
#12974 = CARTESIAN_POINT ( 'NONE',  ( -1.901381477150592358, -2.939880072212064377, 0.05875302977771206664 ) ) ;
#12975 = CARTESIAN_POINT ( 'NONE',  ( -0.03886060139087894189, 0.07874015748031495954, -0.08219815605944147396 ) ) ;
#12976 = VECTOR ( 'NONE', #2114, 39.37007874015748143 ) ;
#12977 = EDGE_CURVE ( 'NONE', #14826, #748, #4882, .T. ) ;
#12978 = DIRECTION ( 'NONE',  ( 0.000000000000000000, 0.000000000000000000, 1.000000000000000000 ) ) ;
#12979 = FACE_OUTER_BOUND ( 'NONE', #10720, .T. ) ;
#12980 = PLANE ( 'NONE',  #2858 ) ;
#12981 = CIRCLE ( 'NONE', #14981, 0.003937007874015749712 ) ;
#12982 = EDGE_CURVE ( 'NONE', #6020, #6007, #10146, .T. ) ;
#12983 = FACE_OUTER_BOUND ( 'NONE', #763, .T. ) ;
#12984 = LENGTH_MEASURE_WITH_UNIT ( LENGTH_MEASURE( 0.02539999999999999897 ), #55 );
#12985 = ORIENTED_EDGE ( 'NONE', *, *, #11437, .F. ) ;
#12986 = EDGE_CURVE ( 'NONE', #14723, #2263, #6366, .T. ) ;
#12987 = EDGE_LOOP ( 'NONE', ( #9948, #4751 ) ) ;
#12988 = ORIENTED_EDGE ( 'NONE', *, *, #6646, .F. ) ;
#12989 = ORIENTED_EDGE ( 'NONE', *, *, #7024, .F. ) ;
#12990 = ADVANCED_FACE ( 'NONE', ( #11663 ), #3891, .T. ) ;
#12991 = CARTESIAN_POINT ( 'NONE',  ( 0.09842519685044814892, -0.2952755905511811330, -0.4190977005962941426 ) ) ;
#12992 = CARTESIAN_POINT ( 'NONE',  ( -1.180847381051866485, 0.3433074774306730803, 0.03937007874015747977 ) ) ;
#12993 = CARTESIAN_POINT ( 'NONE',  ( -0.04507696108106434146, -0.1650637432014245287, -0.05202626060216886811 ) ) ;
#12994 = FACE_OUTER_BOUND ( 'NONE', #5469, .T. ) ;
#12995 = DIRECTION ( 'NONE',  ( 0.000000000000000000, 0.000000000000000000, 1.000000000000000000 ) ) ;
#12996 = ORIENTED_EDGE ( 'NONE', *, *, #12039, .F. ) ;
#12997 = DIRECTION ( 'NONE',  ( 1.000000000000000000, 0.000000000000000000, 0.000000000000000000 ) ) ;
#12998 = DIRECTION ( 'NONE',  ( -0.000000000000000000, -0.000000000000000000, 1.000000000000000000 ) ) ;
#12999 = ORIENTED_EDGE ( 'NONE', *, *, #1310, .T. ) ;
#13000 = ORIENTED_EDGE ( 'NONE', *, *, #15154, .F. ) ;
#13001 = ADVANCED_FACE ( 'NONE', ( #8042 ), #9303, .T. ) ;
#13002 = ORIENTED_EDGE ( 'NONE', *, *, #12396, .T. ) ;
#13003 = ADVANCED_FACE ( 'NONE', ( #10553 ), #5119, .T. ) ;
#13004 = DIRECTION ( 'NONE',  ( 0.8660254037844385966, 0.000000000000000000, -0.5000000000000000000 ) ) ;
#13005 = EDGE_CURVE ( 'NONE', #7918, #2233, #15141, .T. ) ;
#13006 = DIRECTION ( 'NONE',  ( -1.000000000000000000, -0.000000000000000000, -3.973232667114495301E-16 ) ) ;
#13007 = FACE_OUTER_BOUND ( 'NONE', #7, .T. ) ;
#13008 = FACE_OUTER_BOUND ( 'NONE', #11271, .T. ) ;
#13009 = CARTESIAN_POINT ( 'NONE',  ( 0.000000000000000000, 0.5511811023622046335, 0.000000000000000000 ) ) ;
#13010 = CARTESIAN_POINT ( 'NONE',  ( -1.916695816424315746, -2.827605297880910751, 0.1689279957868018711 ) ) ;
#13011 = ORIENTED_EDGE ( 'NONE', *, *, #7798, .T. ) ;
#13012 = DIRECTION ( 'NONE',  ( -0.000000000000000000, -1.000000000000000000, -0.000000000000000000 ) ) ;
#13013 = CARTESIAN_POINT ( 'NONE',  ( 0.2652685895082805834, -0.4881889763779528324, 0.03495519865525829883 ) ) ;
#13014 = DIRECTION ( 'NONE',  ( 1.000000000000000000, 0.000000000000000000, 0.000000000000000000 ) ) ;
#13015 = CARTESIAN_POINT ( 'NONE',  ( -1.606327126723951615, 0.09914643767337930069, 0.06529511858635557442 ) ) ;
#13016 = ORIENTED_EDGE ( 'NONE', *, *, #2731, .F. ) ;
#13017 = ORIENTED_EDGE ( 'NONE', *, *, #10654, .T. ) ;
#13018 = EDGE_LOOP ( 'NONE', ( #8099, #10530, #42, #2414 ) ) ;
#13019 = EDGE_LOOP ( 'NONE', ( #7005, #13965, #5014, #5264, #14411, #11915 ) ) ;
#13020 = VERTEX_POINT ( 'NONE', #8133 ) ;
#13021 = CARTESIAN_POINT ( 'NONE',  ( -0.02063990244551198311, 0.1734013470568572801, -3.760128896581743291E-13 ) ) ;
#13022 = CARTESIAN_POINT ( 'NONE',  ( -0.06278592661683282672, 1.038795580266492768, -0.5877247716201635663 ) ) ;
#13023 = FACE_OUTER_BOUND ( 'NONE', #14142, .T. ) ;
#13024 = CONTEXT_DEPENDENT_SHAPE_REPRESENTATION ( #1701, #13556 ) ;
#13025 = FACE_OUTER_BOUND ( 'NONE', #5142, .T. ) ;
#13026 = DIRECTION ( 'NONE',  ( -0.4999999999999919509, 0.000000000000000000, 0.8660254037844432595 ) ) ;
#13027 = ORIENTED_EDGE ( 'NONE', *, *, #14198, .F. ) ;
#13028 = CARTESIAN_POINT ( 'NONE',  ( 0.3492731901935992034, -0.2952755905511811330, 0.3198506632839551167 ) ) ;
#13029 = DIRECTION ( 'NONE',  ( -4.336808689942014285E-16, 0.000000000000000000, 1.000000000000000000 ) ) ;
#13030 = CARTESIAN_POINT ( 'NONE',  ( -1.137795275590550936, 0.000000000000000000, 0.02952755905511811330 ) ) ;
#13031 = CARTESIAN_POINT ( 'NONE',  ( 0.5860051159906327634, -0.003937007874015747977, 0.1591122789105294533 ) ) ;
#13032 = ORIENTED_EDGE ( 'NONE', *, *, #7746, .F. ) ;
#13033 = FACE_OUTER_BOUND ( 'NONE', #6179, .T. ) ;
#13034 = ORIENTED_EDGE ( 'NONE', *, *, #2258, .T. ) ;
#13035 = ORIENTED_EDGE ( 'NONE', *, *, #9935, .T. ) ;
#13036 = EDGE_CURVE ( 'NONE', #12161, #3451, #11572, .T. ) ;
#13037 = ORIENTED_EDGE ( 'NONE', *, *, #4302, .F. ) ;
#13038 = CARTESIAN_POINT ( 'NONE',  ( -0.5860051159906336515, -0.003937007874015747977, 0.1591122789105256508 ) ) ;
#13039 = EDGE_CURVE ( 'NONE', #563, #2898, #10861, .T. ) ;
#13040 = CARTESIAN_POINT ( 'NONE',  ( 0.000000000000000000, 0.5826771653543306728, 0.000000000000000000 ) ) ;
#13041 = CARTESIAN_POINT ( 'NONE',  ( -1.900032110109137307, -2.943588721549657006, -0.04688266410269418399 ) ) ;
#13042 =( NAMED_UNIT ( * ) SI_UNIT ( $, .STERADIAN. ) SOLID_ANGLE_UNIT ( ) );
#13043 = PRODUCT_DEFINITION_SHAPE ( 'NONE', 'NONE',  #15474 ) ;
#13044 = CARTESIAN_POINT ( 'NONE',  ( -1.580080891953811850, 0.1020406297922293037, -0.07529375917861416689 ) ) ;
#13045 = ADVANCED_FACE ( 'NONE', ( #7028 ), #12653, .T. ) ;
#13046 = CARTESIAN_POINT ( 'NONE',  ( -1.387704745771440429, -0.02010536753476150837, 0.03937007874015747977 ) ) ;
#13047 = CARTESIAN_POINT ( 'NONE',  ( -2.080881322745466999, -1.632190302820504479, -0.08366141732283423338 ) ) ;
#13048 = FACE_OUTER_BOUND ( 'NONE', #9946, .T. ) ;
#13049 = EDGE_LOOP ( 'NONE', ( #11302, #9922 ) ) ;
#13050 = ORIENTED_EDGE ( 'NONE', *, *, #13512, .F. ) ;
#13051 = ORIENTED_EDGE ( 'NONE', *, *, #14016, .F. ) ;
#13052 = ORIENTED_EDGE ( 'NONE', *, *, #8024, .F. ) ;
#13053 = ADVANCED_FACE ( 'NONE', ( #1080 ), #6712, .T. ) ;
#13054 = B_SPLINE_CURVE_WITH_KNOTS ( 'NONE', 3,
 ( #4578, #9367, #1063, #10616 ),
 .UNSPECIFIED., .F., .F.,
 ( 4, 4 ),
 ( 0.000000000000000000, 0.0006024839870383029905 ),
 .UNSPECIFIED. ) ;
#13055 = ADVANCED_FACE ( 'NONE', ( #14313 ), #5043, .T. ) ;
#13056 = DIRECTION ( 'NONE',  ( -0.000000000000000000, -0.000000000000000000, -1.000000000000000000 ) ) ;
#13057 = EDGE_CURVE ( 'NONE', #14663, #2421, #10717, .T. ) ;
#13058 = CARTESIAN_POINT ( 'NONE',  ( -1.572611271869832184, 0.1123963381039306264, -0.05997718891474942970 ) ) ;
#13059 = DIRECTION ( 'NONE',  ( 0.000000000000000000, 1.000000000000000000, 0.000000000000000000 ) ) ;
#13060 = CARTESIAN_POINT ( 'NONE',  ( -1.181102362204724310, -0.1279527559055117225, 0.02559055118110236185 ) ) ;
#13061 = ORIENTED_EDGE ( 'NONE', *, *, #11325, .T. ) ;
#13062 = DIRECTION ( 'NONE',  ( 0.000000000000000000, 0.000000000000000000, 1.000000000000000000 ) ) ;
#13063 = DIRECTION ( 'NONE',  ( -3.973232667114494807E-16, 0.000000000000000000, 1.000000000000000000 ) ) ;
#13064 = DIRECTION ( 'NONE',  ( -0.000000000000000000, -1.000000000000000000, -0.000000000000000000 ) ) ;
#13065 = DIMENSIONAL_EXPONENTS ( 1.000000000000000000, 0.000000000000000000, 0.000000000000000000, 0.000000000000000000, 0.000000000000000000, 0.000000000000000000, 0.000000000000000000 ) ;
#13066 = ORIENTED_EDGE ( 'NONE', *, *, #15154, .T. ) ;
#13067 = ORIENTED_EDGE ( 'NONE', *, *, #8727, .T. ) ;
#13068 = EDGE_LOOP ( 'NONE', ( #14825, #14551, #5927, #15112 ) ) ;
#13069 = DIRECTION ( 'NONE',  ( -0.000000000000000000, 0.000000000000000000, 1.000000000000000000 ) ) ;
#13070 = CARTESIAN_POINT ( 'NONE',  ( -1.944249365573698540, -2.934812813689591682, 0.02858372338952079941 ) ) ;
#13071 = CARTESIAN_POINT ( 'NONE',  ( -2.755905511811024056, -2.772329397582842248, 0.000000000000000000 ) ) ;
#13072 = CARTESIAN_POINT ( 'NONE',  ( -1.950280692371897384, -2.878718452480370615, -0.1421344132345661593 ) ) ;
#13073 = EDGE_CURVE ( 'NONE', #6404, #7200, #13156, .T. ) ;
#13074 = DIRECTION ( 'NONE',  ( 0.000000000000000000, 0.000000000000000000, -1.000000000000000000 ) ) ;
#13075 = CARTESIAN_POINT ( 'NONE',  ( -2.116009644208461271, -1.821148055095885399, 0.1033464566929130357 ) ) ;
#13076 = ORIENTED_EDGE ( 'NONE', *, *, #12395, .F. ) ;
#13077 = CARTESIAN_POINT ( 'NONE',  ( -1.969122886354301327, -2.872755761241831518, -0.1273454318878232960 ) ) ;
#13078 = DIRECTION ( 'NONE',  ( 0.5000000000000002220, 0.000000000000000000, -0.8660254037844384856 ) ) ;
#13079 = CARTESIAN_POINT ( 'NONE',  ( 0.000000000000000000, 1.653543307086614567, 0.000000000000000000 ) ) ;
#13080 = DIRECTION ( 'NONE',  ( -0.8660254037844431485, 0.000000000000000000, -0.4999999999999918954 ) ) ;
#13081 = ORIENTED_EDGE ( 'NONE', *, *, #5187, .T. ) ;
#13082 = ADVANCED_FACE ( 'NONE', ( #2639 ), #7412, .T. ) ;
#13083 = CIRCLE ( 'NONE', #14584, 0.007874015748031516770 ) ;
#13084 = VECTOR ( 'NONE', #10790, 39.37007874015748143 ) ;
#13085 = ORIENTED_EDGE ( 'NONE', *, *, #3831, .T. ) ;
#13086 = AXIS2_PLACEMENT_3D ( 'NONE', #6306, #392, #9956 ) ;
#13087 = ORIENTED_EDGE ( 'NONE', *, *, #10612, .F. ) ;
#13088 = CARTESIAN_POINT ( 'NONE',  ( 0.1618514667033794374, -0.1023622047244094474, 0.2122517380126066888 ) ) ;
#13089 = CARTESIAN_POINT ( 'NONE',  ( 0.06692913385826772255, 0.000000000000000000, -0.5946706712680680518 ) ) ;
#13090 = FACE_OUTER_BOUND ( 'NONE', #15221, .T. ) ;
#13091 = CARTESIAN_POINT ( 'NONE',  ( -0.06438893898759022461, 1.037114193080275637, -0.5870328364109900221 ) ) ;
#13092 = LINE ( 'NONE', #3624, #1115 ) ;
#13093 = DIRECTION ( 'NONE',  ( -0.9387676358163957735, 0.3445509047204710629, 1.288839711614000126E-12 ) ) ;
#13094 = TOROIDAL_SURFACE ( 'NONE', #6316, 0.007874015748031495954, 0.003937007874015747977 ) ;
#13095 = DIRECTION ( 'NONE',  ( 0.8660254037844387076, 0.000000000000000000, -0.4999999999999999445 ) ) ;
#13096 = VERTEX_POINT ( 'NONE', #2548 ) ;
#13097 = CARTESIAN_POINT ( 'NONE',  ( -1.576192857444074225, 0.1076040293810619497, -0.06348264010178604477 ) ) ;
#13098 = AXIS2_PLACEMENT_3D ( 'NONE', #8869, #13278, #13877 ) ;
#13099 = TOROIDAL_SURFACE ( 'NONE', #6319, 0.7007874015748031260, 0.007874015748031495954 ) ;
#13100 = DIRECTION ( 'NONE',  ( 0.000000000000000000, -0.000000000000000000, -1.000000000000000000 ) ) ;
#13101 =( CONVERSION_BASED_UNIT ( 'INCH', #11863 ) LENGTH_UNIT ( ) NAMED_UNIT ( #11672 ) );
#13102 = EDGE_CURVE ( 'NONE', #10393, #14453, #3669, .T. ) ;
#13103 =( LENGTH_UNIT ( ) NAMED_UNIT ( * ) SI_UNIT ( $, .METRE. ) );
#13104 = ORIENTED_EDGE ( 'NONE', *, *, #693, .T. ) ;
#13105 = EDGE_LOOP ( 'NONE', ( #2912, #15123, #8285, #2646 ) ) ;
#13107 = ORIENTED_EDGE ( 'NONE', *, *, #14776, .T. ) ;
#13106 = AXIS2_PLACEMENT_3D ( 'NONE', #10613, #11487, #753 ) ;
#13108 = AXIS2_PLACEMENT_3D ( 'NONE', #6206, #8332, #14294 ) ;
#13109 = ORIENTED_EDGE ( 'NONE', *, *, #6447, .T. ) ;
#13110 = AXIS2_PLACEMENT_3D ( 'NONE', #6954, #2303, #2388 ) ;
#13111 = ORIENTED_EDGE ( 'NONE', *, *, #2440, .F. ) ;
#13112 = TOROIDAL_SURFACE ( 'NONE', #6595, 0.7007874015748031260, 0.007874015748031495954 ) ;
#13113 = DIRECTION ( 'NONE',  ( 1.000000000000000000, 0.000000000000000000, 0.000000000000000000 ) ) ;
#13114 = AXIS2_PLACEMENT_3D ( 'NONE', #1519, #14765, #6271 ) ;
#13115 = DIRECTION ( 'NONE',  ( 0.000000000000000000, 1.000000000000000000, 0.000000000000000000 ) ) ;
#13116 = CARTESIAN_POINT ( 'NONE',  ( -1.911437664849721108, -2.911761458588945750, 0.1099279165421168103 ) ) ;
#13117 = CARTESIAN_POINT ( 'NONE',  ( 0.1181102362204670825, 37.37889961492984980, -0.8267716535433132785 ) ) ;
#13118 = CARTESIAN_POINT ( 'NONE',  ( -2.182693454834259139, -1.630005269948474389, 0.08366141732283424726 ) ) ;
#13119 = CARTESIAN_POINT ( 'NONE',  ( -0.1618514667033796040, -0.4881889763779528324, 0.2122517380126066888 ) ) ;
#13120 = DIRECTION ( 'NONE',  ( 0.000000000000000000, 1.000000000000000000, 0.000000000000000000 ) ) ;
#13121 = AXIS2_PLACEMENT_3D ( 'NONE', #13468, #7505, #2795 ) ;
#13122 = VECTOR ( 'NONE', #14006, 39.37007874015748143 ) ;
#13123 = CIRCLE ( 'NONE', #1358, 0.1279527559055117780 ) ;
#13124 = AXIS2_PLACEMENT_3D ( 'NONE', #14090, #718, #949 ) ;
#13125 = CARTESIAN_POINT ( 'NONE',  ( -1.396233373141806400, -0.02565714533840434894, 0.04040313278352580806 ) ) ;
#13126 = DIRECTION ( 'NONE',  ( 0.9162674345903514261, -0.4005670834070318986, 0.000000000000000000 ) ) ;
#13127 = AXIS2_PLACEMENT_3D ( 'NONE', #3054, #11448, #14811 ) ;
#13128 = ADVANCED_FACE ( 'NONE', ( #1245 ), #14918, .T. ) ;
#13129 = VERTEX_POINT ( 'NONE', #65 ) ;
#13130 = EDGE_LOOP ( 'NONE', ( #10418, #11203 ) ) ;
#13131 = VERTEX_POINT ( 'NONE', #3576 ) ;
#13132 = VERTEX_POINT ( 'NONE', #7260 ) ;
#13133 = EDGE_LOOP ( 'NONE', ( #5261, #5916, #14040, #13878 ) ) ;
#13134 = EDGE_CURVE ( 'NONE', #10775, #11599, #4896, .T. ) ;
#13135 = CIRCLE ( 'NONE', #4371, 0.04330708661417331101 ) ;
#13136 = CIRCLE ( 'NONE', #2374, 0.04330708661417331101 ) ;
#13137 = CIRCLE ( 'NONE', #7378, 0.03937007874015751446 ) ;
#13138 = CARTESIAN_POINT ( 'NONE',  ( -0.3441669734936866343, 2.010494531933507467, 0.05905511811023622659 ) ) ;
#13139 = TOROIDAL_SURFACE ( 'NONE', #11914, 0.6614173228346456046, 0.007874015748031495954 ) ;
#13140 = CARTESIAN_POINT ( 'NONE',  ( -1.591501945092674841, 0.08600752902535294120, 0.08366141732283462196 ) ) ;
#13141 = DIRECTION ( 'NONE',  ( 0.4999999999999979461, 0.000000000000000000, 0.8660254037844398178 ) ) ;
#13142 = CARTESIAN_POINT ( 'NONE',  ( 0.6864776960422567242, 1.338582677165354395, 0.4645290592786021633 ) ) ;
#13143 = CARTESIAN_POINT ( 'NONE',  ( 0.05905511811023622659, 1.043307086614173373, -0.5955041639236610118 ) ) ;
#13144 = VERTEX_POINT ( 'NONE', #7325 ) ;
#13145 = CARTESIAN_POINT ( 'NONE',  ( 0.000000000000000000, 0.03149606299212599769, -0.1574803149606299191 ) ) ;
#13146 = DIRECTION ( 'NONE',  ( -0.4999999999999966693, 0.000000000000000000, -0.8660254037844405950 ) ) ;
#13147 = CARTESIAN_POINT ( 'NONE',  ( 0.4307978335858664853, -0.003937007874015747977, 0.4318761856142889766 ) ) ;
#13148 = ADVANCED_FACE ( 'NONE', ( #3808 ), #152, .T. ) ;
#13149 = AXIS2_PLACEMENT_3D ( 'NONE', #6785, #844, #10410 ) ;
#13150 = AXIS2_PLACEMENT_3D ( 'NONE', #13491, #849, #8866 ) ;
#13151 = B_SPLINE_CURVE_WITH_KNOTS ( 'NONE', 3,
 ( #5813, #2470, #8107, #9457, #1293, #12892, #1060, #14372, #11876, #3496, #2302, #8266, #7242, #4667, #13041, #4800, #6933, #10537, #10767, #993, #9286, #8373, #12974, #3645, #5741, #13116, #12033, #15316, #8200, #14230, #7078, #1150, #4576, #10614, #5905, #2164 ),
 .UNSPECIFIED., .F., .F.,
 ( 4, 2, 2, 2, 2, 2, 2, 2, 2, 2, 2, 2, 2, 2, 2, 2, 2, 4 ),
 ( 0.0006024839870383029905, 0.001504406831461554354, 0.002406329675884806042, 0.003308252520308057297, 0.004210175364731308552, 0.005112098209154560674, 0.006014021053577811061, 0.006915943898001062316, 0.007366905320212691413, 0.007817866742424321377, 0.008719789586847579571, 0.009621712431270836030, 0.01052363527569409422, 0.01142555812011735242, 0.01232748096454061061, 0.01322940380896386707, 0.01413132665338712526, 0.01503324949781038346 ),
 .UNSPECIFIED. ) ;
#13152 = EDGE_CURVE ( 'NONE', #7115, #7217, #6892, .T. ) ;
#13153 = AXIS2_PLACEMENT_3D ( 'NONE', #12726, #4311, #9105 ) ;
#13154 = ORIENTED_EDGE ( 'NONE', *, *, #11563, .T. ) ;
#13155 = EDGE_LOOP ( 'NONE', ( #5806, #13804, #3785 ) ) ;
#13156 = CIRCLE ( 'NONE', #15421, 0.1476377952755906775 ) ;
#13157 = ADVANCED_FACE ( 'NONE', ( #2409 ), #12125, .T. ) ;
#13158 = ORIENTED_EDGE ( 'NONE', *, *, #2538, .F. ) ;
#13159 = FACE_OUTER_BOUND ( 'NONE', #12987, .T. ) ;
#13160 = AXIS2_PLACEMENT_3D ( 'NONE', #1847, #12669, #10238 ) ;
#13161 = CARTESIAN_POINT ( 'NONE',  ( -1.925012530255905130, -2.949505661444294269, 0.006211189736853072255 ) ) ;
#13162 = VECTOR ( 'NONE', #4918, 39.37007874015748143 ) ;
#13163 = DIRECTION ( 'NONE',  ( -0.5000000000000039968, 0.000000000000000000, -0.8660254037844362651 ) ) ;
#13164 = CARTESIAN_POINT ( 'NONE',  ( -0.02433043306709228512, -0.1808586691373950950, -0.01162756877077187820 ) ) ;
#13165 = DIRECTION ( 'NONE',  ( -0.3445509047216855913, -0.9387676358159497969, 0.000000000000000000 ) ) ;
#13166 = LINE ( 'NONE', #4706, #3959 ) ;
#13167 = AXIS2_PLACEMENT_3D ( 'NONE', #12192, #13434, #2701 ) ;
#13168 = CARTESIAN_POINT ( 'NONE',  ( -1.925363067542684936, -2.803745874285077821, 0.1746042784463377462 ) ) ;
#13169 = ORIENTED_EDGE ( 'NONE', *, *, #9226, .F. ) ;
#13170 = CARTESIAN_POINT ( 'NONE',  ( -1.943201052682586027, -2.937347917504331996, 0.005536254343342756137 ) ) ;
#13171 = EDGE_CURVE ( 'NONE', #8390, #12616, #7189, .T. ) ;
#13172 = CARTESIAN_POINT ( 'NONE',  ( -0.7455328141524870667, 1.338582677165354395, 0.3622425942647020669 ) ) ;
#13173 = DIRECTION ( 'NONE',  ( 0.000000000000000000, 0.000000000000000000, 1.000000000000000000 ) ) ;
#13174 = EDGE_CURVE ( 'NONE', #4567, #532, #6137, .T. ) ;
#13175 = ORIENTED_EDGE ( 'NONE', *, *, #7165, .F. ) ;
#13176 = VECTOR ( 'NONE', #5338, 39.37007874015748143 ) ;
#13177 = EDGE_CURVE ( 'NONE', #381, #6293, #1649, .T. ) ;
#13178 = PRODUCT_DEFINITION_CONTEXT ( 'detailed design', #8095, 'design' ) ;
#13179 = VERTEX_POINT ( 'NONE', #1474 ) ;
#13180 = AXIS2_PLACEMENT_3D ( 'NONE', #14907, #2991, #10201 ) ;
#13181 = DIRECTION ( 'NONE',  ( -0.000000000000000000, -1.000000000000000000, -0.000000000000000000 ) ) ;
#13182 = DIRECTION ( 'NONE',  ( 0.000000000000000000, 0.000000000000000000, -1.000000000000000000 ) ) ;
#13183 = EDGE_CURVE ( 'NONE', #4234, #14001, #3773, .T. ) ;
#13184 = CARTESIAN_POINT ( 'NONE',  ( -1.399422649241788497, -0.02634252632334466854, 0.07488899955401198683 ) ) ;
#13185 = CARTESIAN_POINT ( 'NONE',  ( -0.1618514667033796040, -0.4921259842519685179, 0.2161887458866224576 ) ) ;
#13186 = FACE_OUTER_BOUND ( 'NONE', #15289, .T. ) ;
#13187 = TOROIDAL_SURFACE ( 'NONE', #10683, 0.5984251968503937480, 0.007874015748031495954 ) ;
#13188 = DIRECTION ( 'NONE',  ( 0.000000000000000000, 0.000000000000000000, 1.000000000000000000 ) ) ;
#13189 = ORIENTED_EDGE ( 'NONE', *, *, #9028, .T. ) ;
#13190 = CARTESIAN_POINT ( 'NONE',  ( -1.580080891959645850, 0.1020406297963854930, -0.07533316186190673613 ) ) ;
#13191 = CARTESIAN_POINT ( 'NONE',  ( -0.2613315816341005848, -0.4921259842519685179, 0.03601011673560078341 ) ) ;
#13192 = AXIS2_PLACEMENT_3D ( 'NONE', #11433, #6637, #12828 ) ;
#13193 = CARTESIAN_POINT ( 'NONE',  ( -0.4141303577462134844, -0.2952755905511811330, 0.1209005806194722171 ) ) ;
#13194 = SURFACE_STYLE_FILL_AREA ( #3248 ) ;
#13195 = CIRCLE ( 'NONE', #14943, 0.003937007874015761855 ) ;
#13196 = EDGE_LOOP ( 'NONE', ( #7162, #13459, #10346, #15181 ) ) ;
#13197 = ORIENTED_EDGE ( 'NONE', *, *, #4166, .T. ) ;
#13198 = AXIS2_PLACEMENT_3D ( 'NONE', #4934, #2500, #1326 ) ;
#13199 = EDGE_CURVE ( 'NONE', #11540, #14826, #11925, .T. ) ;
#13200 = ORIENTED_EDGE ( 'NONE', *, *, #14318, .F. ) ;
#13201 = VECTOR ( 'NONE', #13705, 39.37007874015748143 ) ;
#13202 = ORIENTED_EDGE ( 'NONE', *, *, #12734, .F. ) ;
#13203 = DIRECTION ( 'NONE',  ( -1.000000000000000000, -0.000000000000000000, -3.476578583725179813E-16 ) ) ;
#13204 = AXIS2_PLACEMENT_3D ( 'NONE', #14251, #11819, #232 ) ;
#13205 = EDGE_CURVE ( 'NONE', #11006, #6292, #8907, .T. ) ;
#13206 = DIRECTION ( 'NONE',  ( 0.000000000000000000, 0.000000000000000000, -1.000000000000000000 ) ) ;
#13207 = DIRECTION ( 'NONE',  ( -0.4999999999999966693, 0.000000000000000000, 0.8660254037844405950 ) ) ;
#13208 = DIRECTION ( 'NONE',  ( 0.2084205441254113333, 0.9706086590632821975, -0.1203316572554560260 ) ) ;
#13209 = VECTOR ( 'NONE', #8951, 39.37007874015748143 ) ;
#13210 = DIRECTION ( 'NONE',  ( 0.000000000000000000, 0.000000000000000000, 1.000000000000000000 ) ) ;
#13211 = DIRECTION ( 'NONE',  ( -0.000000000000000000, -0.000000000000000000, -1.000000000000000000 ) ) ;
#13212 = CIRCLE ( 'NONE', #11719, 0.003937007874015741038 ) ;
#13213 = DIRECTION ( 'NONE',  ( -0.000000000000000000, 1.000000000000000000, 0.000000000000000000 ) ) ;
#13214 = CARTESIAN_POINT ( 'NONE',  ( 0.1259842519685039353, 2.440944881889763884, 0.04724409448818898266 ) ) ;
#13215 = PRESENTATION_LAYER_ASSIGNMENT (  '', '', ( #2947 ) ) ;
#13216 = ORIENTED_EDGE ( 'NONE', *, *, #14198, .T. ) ;
#13217 = ORIENTED_EDGE ( 'NONE', *, *, #9464, .T. ) ;
#13218 = CIRCLE ( 'NONE', #10466, 0.1574803149606299191 ) ;
#13219 = DIRECTION ( 'NONE',  ( 0.000000000000000000, 0.000000000000000000, -1.000000000000000000 ) ) ;
#13220 = DIRECTION ( 'NONE',  ( 0.8660254037844405950, 0.000000000000000000, 0.4999999999999967804 ) ) ;
#13221 = AXIS2_PLACEMENT_3D ( 'NONE', #10339, #5002, #1423 ) ;
#13222 = DIRECTION ( 'NONE',  ( 1.000000000000000000, 0.000000000000000000, 0.000000000000000000 ) ) ;
#13223 = DIRECTION ( 'NONE',  ( -0.000000000000000000, -1.000000000000000000, -0.000000000000000000 ) ) ;
#13224 = CARTESIAN_POINT ( 'NONE',  ( -0.3441669734936866343, 2.010494531933507467, 0.03937007874015747977 ) ) ;
#13225 = FACE_OUTER_BOUND ( 'NONE', #5451, .T. ) ;
#13226 = CARTESIAN_POINT ( 'NONE',  ( 0.000000000000000000, 1.606299212598425674, 0.000000000000000000 ) ) ;
#13227 = DIRECTION ( 'NONE',  ( 1.000000000000000000, -1.734723475976802677E-14, 0.000000000000000000 ) ) ;
#13228 = DIRECTION ( 'NONE',  ( 0.4999999999999979461, -0.000000000000000000, 0.8660254037844398178 ) ) ;
#13229 = AXIS2_PLACEMENT_3D ( 'NONE', #246, #313, #12150 ) ;
#13230 = ORIENTED_EDGE ( 'NONE', *, *, #4353, .T. ) ;
#13231 = EDGE_LOOP ( 'NONE', ( #3748, #8841, #3984, #6255 ) ) ;
#13232 = VERTEX_POINT ( 'NONE', #11645 ) ;
#13233 = DIRECTION ( 'NONE',  ( -0.000000000000000000, -1.000000000000000000, -0.000000000000000000 ) ) ;
#13234 = EDGE_CURVE ( 'NONE', #10253, #13441, #2151, .T. ) ;
#13235 = EDGE_CURVE ( 'NONE', #7381, #14387, #13993, .T. ) ;
#13236 = CYLINDRICAL_SURFACE ( 'NONE', #13366, 0.003937007874015749712 ) ;
#13237 = CARTESIAN_POINT ( 'NONE',  ( 0.9851651268172137987, -1.725292181286280480, -0.1033464566929129524 ) ) ;
#13238 = DIRECTION ( 'NONE',  ( -0.000000000000000000, 0.000000000000000000, 1.000000000000000000 ) ) ;
#13239 = FACE_OUTER_BOUND ( 'NONE', #4881, .T. ) ;
#13240 = CARTESIAN_POINT ( 'NONE',  ( -2.100501784635051550, -1.630597114118274238, 0.1033464566929129663 ) ) ;
#13241 = VERTEX_POINT ( 'NONE', #917 ) ;
#13242 = DIRECTION ( 'NONE',  ( -3.973232667114495301E-16, 0.000000000000000000, 1.000000000000000000 ) ) ;
#13243 = EDGE_CURVE ( 'NONE', #14035, #5216, #3654, .T. ) ;
#13244 = CARTESIAN_POINT ( 'NONE',  ( -1.574484809660440021, 0.1100025355989264070, 0.06175692796217654990 ) ) ;
#13245 = DIRECTION ( 'NONE',  ( -1.000000000000000000, 0.000000000000000000, 0.000000000000000000 ) ) ;
#13246 = ORIENTED_EDGE ( 'NONE', *, *, #9611, .F. ) ;
#13247 = ORIENTED_EDGE ( 'NONE', *, *, #9538, .F. ) ;
#13248 = ORIENTED_EDGE ( 'NONE', *, *, #10757, .T. ) ;
#13249 = ADVANCED_FACE ( 'NONE', ( #7118 ), #11879, .T. ) ;
#13250 = B_SPLINE_CURVE_WITH_KNOTS ( 'NONE', 3,
 ( #14008, #5289, #7895, #8932 ),
 .UNSPECIFIED., .F., .F.,
 ( 4, 4 ),
 ( -2.828444569873223727E-06, 0.0002461255424396390835 ),
 .UNSPECIFIED. ) ;
#13251 = FACE_OUTER_BOUND ( 'NONE', #9736, .T. ) ;
#13252 = EDGE_CURVE ( 'NONE', #1254, #14240, #3327, .T. ) ;
#13253 = CARTESIAN_POINT ( 'NONE',  ( -1.415645031250719388, -0.01001692594509011672, 0.06639602688116504059 ) ) ;
#13254 = CARTESIAN_POINT ( 'NONE',  ( -1.078976767140036319, 0.8059172436903675463, 0.05905511811023622659 ) ) ;
#13255 = CARTESIAN_POINT ( 'NONE',  ( -0.06473829668901623369, 0.07239639532902288066, -0.04482148303916006632 ) ) ;
#13256 = DIRECTION ( 'NONE',  ( 0.000000000000000000, 1.000000000000000000, 0.000000000000000000 ) ) ;
#13257 = DIRECTION ( 'NONE',  ( -0.000000000000000000, -1.000000000000000000, -0.000000000000000000 ) ) ;
#13258 = ORIENTED_EDGE ( 'NONE', *, *, #10585, .T. ) ;
#13259 = CARTESIAN_POINT ( 'NONE',  ( -1.592259916642329465, 0.1190110821473790575, -0.06350111023902997587 ) ) ;
#13260 = EDGE_CURVE ( 'NONE', #8290, #12501, #9151, .T. ) ;
#13261 = ADVANCED_FACE ( 'NONE', ( #5815 ), #11735, .F. ) ;
#13262 = CARTESIAN_POINT ( 'NONE',  ( 8.148240514011916814E-17, 0.5511811023622046335, -0.6614173228346456046 ) ) ;
#13263 = CARTESIAN_POINT ( 'NONE',  ( -0.004688298860636740291, -0.1607931678657651686, 0.008473975361459438679 ) ) ;
#13264 = DIRECTION ( 'NONE',  ( -0.000000000000000000, -1.000000000000000000, -0.000000000000000000 ) ) ;
#13265 = ORIENTED_EDGE ( 'NONE', *, *, #7132, .F. ) ;
#13266 = VERTEX_POINT ( 'NONE', #8336 ) ;
#13267 = ORIENTED_EDGE ( 'NONE', *, *, #1089, .T. ) ;
#13268 = ORIENTED_EDGE ( 'NONE', *, *, #11997, .F. ) ;
#13269 = DIRECTION ( 'NONE',  ( 1.000000000000000000, 0.000000000000000000, 0.000000000000000000 ) ) ;
#13270 = DIRECTION ( 'NONE',  ( 0.000000000000000000, -0.000000000000000000, 1.000000000000000000 ) ) ;
#13271 = CARTESIAN_POINT ( 'NONE',  ( -0.4342073824196659437, -0.09448818897637796532, 0.4299076816772785525 ) ) ;
#13272 = DIRECTION ( 'NONE',  ( 0.4356761836762389484, 0.8642424528470444844, 0.2515377619249882235 ) ) ;
#13273 = FACE_OUTER_BOUND ( 'NONE', #1248, .T. ) ;
#13274 = DIRECTION ( 'NONE',  ( 0.8660254037844383745, 0.000000000000000000, -0.5000000000000004441 ) ) ;
#13275 = DIRECTION ( 'NONE',  ( 0.000000000000000000, -1.000000000000000000, 0.000000000000000000 ) ) ;
#13276 = EDGE_CURVE ( 'NONE', #9540, #253, #10468, .T. ) ;
#13277 = CARTESIAN_POINT ( 'NONE',  ( 0.05905511811029064834, -0.09448818897637796532, -0.5909884645248143498 ) ) ;
#13278 = DIRECTION ( 'NONE',  ( -0.000000000000000000, -0.000000000000000000, -1.000000000000000000 ) ) ;
#13279 = DIRECTION ( 'NONE',  ( 0.000000000000000000, 0.000000000000000000, 1.000000000000000000 ) ) ;
#13280 = ORIENTED_EDGE ( 'NONE', *, *, #8982, .T. ) ;
#13281 = ADVANCED_FACE ( 'NONE', ( #3560 ), #12665, .F. ) ;
#13282 = ORIENTED_EDGE ( 'NONE', *, *, #2672, .F. ) ;
#13283 = VERTEX_POINT ( 'NONE', #7013 ) ;
#13284 =( BOUNDED_CURVE ( )  B_SPLINE_CURVE ( 3, ( #2550, #8814, #6381, #2722 ),
 .UNSPECIFIED., .F., .T. ) 
 B_SPLINE_CURVE_WITH_KNOTS ( ( 4, 4 ),
 ( 1.570796326794896780, 4.712388980384689674 ),
 .UNSPECIFIED. ) 
 CURVE ( )  GEOMETRIC_REPRESENTATION_ITEM ( )  RATIONAL_B_SPLINE_CURVE ( ( 1.000000000000000000, 0.3333333333333333703, 0.3333333333333333703, 1.000000000000000000 ) ) 
 REPRESENTATION_ITEM ( '' )  );
#13285 = FACE_OUTER_BOUND ( 'NONE', #14027, .T. ) ;
#13286 = CARTESIAN_POINT ( 'NONE',  ( -1.309055118110236116, 0.000000000000000000, 0.02559055118110236185 ) ) ;
#13287 = FACE_OUTER_BOUND ( 'NONE', #12179, .T. ) ;
#13288 = DIRECTION ( 'NONE',  ( 0.5000000000000035527, 0.000000000000000000, -0.8660254037844365982 ) ) ;
#13289 = CARTESIAN_POINT ( 'NONE',  ( 0.4307978335858664853, -0.09448818897637796532, 0.4318761856142889766 ) ) ;
#13290 = DIRECTION ( 'NONE',  ( 0.000000000000000000, 2.212657494868377674E-16, 1.000000000000000000 ) ) ;
#13291 = CARTESIAN_POINT ( 'NONE',  ( 0.000000000000000000, 2.161417322834645827, 0.000000000000000000 ) ) ;
#13292 = DIRECTION ( 'NONE',  ( -1.000000000000000000, -0.000000000000000000, -3.476578583725179813E-16 ) ) ;
#13293 = DIRECTION ( 'NONE',  ( -0.000000000000000000, -0.000000000000000000, -1.000000000000000000 ) ) ;
#13294 = ORIENTED_EDGE ( 'NONE', *, *, #1214, .F. ) ;
#13295 = ORIENTED_EDGE ( 'NONE', *, *, #11368, .F. ) ;
#13296 = VERTEX_POINT ( 'NONE', #4505 ) ;
#13297 = ORIENTED_EDGE ( 'NONE', *, *, #8852, .T. ) ;
#13298 = CARTESIAN_POINT ( 'NONE',  ( 6.750021727583836750E-17, 1.622047244094488638, 0.5511811023622046335 ) ) ;
#13299 = DIRECTION ( 'NONE',  ( 0.000000000000000000, -1.000000000000000000, -0.000000000000000000 ) ) ;
#13300 = DIRECTION ( 'NONE',  ( -1.000000000000000000, 0.000000000000000000, 0.000000000000000000 ) ) ;
#13301 = DIRECTION ( 'NONE',  ( -0.000000000000000000, -1.000000000000000000, -0.000000000000000000 ) ) ;
#13302 = CARTESIAN_POINT ( 'NONE',  ( -2.073879752373330110, -2.575632606091952326, 0.1529717276801960957 ) ) ;
#13303 = CARTESIAN_POINT ( 'NONE',  ( -1.190198933766852374, 0.3259758027579606199, 0.05905511811023622659 ) ) ;
#13304 = CARTESIAN_POINT ( 'NONE',  ( -1.946192867917152292, -2.743611295743889844, 0.1749236412511669947 ) ) ;
#13305 = VERTEX_POINT ( 'NONE', #13119 ) ;
#13306 = CARTESIAN_POINT ( 'NONE',  ( 0.000000000000000000, 0.04724409448818898960, -0.5511811023622046335 ) ) ;
#13307 = CYLINDRICAL_SURFACE ( 'NONE', #1962, 0.07874015748031495954 ) ;
#13308 = ORIENTED_EDGE ( 'NONE', *, *, #13260, .T. ) ;
#13309 = ADVANCED_FACE ( 'NONE', ( #4672 ), #9461, .F. ) ;
#13310 = EDGE_LOOP ( 'NONE', ( #14524, #12302, #9252, #2669 ) ) ;
#13311 = EDGE_CURVE ( 'NONE', #11994, #10116, #12910, .T. ) ;
#13312 = ORIENTED_EDGE ( 'NONE', *, *, #1680, .F. ) ;
#13313 = DIRECTION ( 'NONE',  ( -1.000000000000000000, 0.000000000000000000, 0.000000000000000000 ) ) ;
#13314 = EDGE_CURVE ( 'NONE', #5035, #10983, #898, .T. ) ;
#13315 = CARTESIAN_POINT ( 'NONE',  ( 0.08413922508867374694, 0.06963377358823465146, -0.006254882657694913091 ) ) ;
#13316 = DIRECTION ( 'NONE',  ( -0.000000000000000000, -1.000000000000000000, -0.000000000000000000 ) ) ;
#13317 = CARTESIAN_POINT ( 'NONE',  ( 0.06692913385832209572, -0.1023622047244094474, -0.2377126739437405434 ) ) ;
#13318 = CONTEXT_DEPENDENT_SHAPE_REPRESENTATION ( #5077, #2281 ) ;
#13319 = DIRECTION ( 'NONE',  ( 0.000000000000000000, 0.000000000000000000, -1.000000000000000000 ) ) ;
#13320 = DIRECTION ( 'NONE',  ( -0.9995479251422038081, 0.03006568382583900759, 0.000000000000000000 ) ) ;
#13321 = DIRECTION ( 'NONE',  ( 0.5000000000000245359, -0.000000000000000000, 0.8660254037844243857 ) ) ;
#13322 = ORIENTED_EDGE ( 'NONE', *, *, #13183, .F. ) ;
#13323 = CARTESIAN_POINT ( 'NONE',  ( -1.590519080053534484, 0.1214231549357164819, -0.06175753274851653041 ) ) ;
#13324 = DIRECTION ( 'NONE',  ( -0.5000000000000001110, 0.000000000000000000, 0.8660254037844387076 ) ) ;
#13325 = DIRECTION ( 'NONE',  ( -0.8660254037844405950, 0.000000000000000000, 0.4999999999999966693 ) ) ;
#13326 = AXIS2_PLACEMENT_3D ( 'NONE', #15469, #3349, #5692 ) ;
#13327 = CARTESIAN_POINT ( 'NONE',  ( -0.002500327830563101039, -0.1605493263772690415, 0.000000000000000000 ) ) ;
#13328 = AXIS2_PLACEMENT_3D ( 'NONE', #13592, #12582, #2866 ) ;
#13329 = DIRECTION ( 'NONE',  ( -1.000000000000000000, 0.000000000000000000, 0.000000000000000000 ) ) ;
#13330 = EDGE_CURVE ( 'NONE', #14199, #2506, #7906, .T. ) ;
#13331 = EDGE_CURVE ( 'NONE', #1797, #4234, #387, .T. ) ;
#13332 = ORIENTED_EDGE ( 'NONE', *, *, #7495, .F. ) ;
#13333 = ORIENTED_EDGE ( 'NONE', *, *, #2258, .F. ) ;
#13334 = ORIENTED_EDGE ( 'NONE', *, *, #9016, .T. ) ;
#13335 = ORIENTED_EDGE ( 'NONE', *, *, #36, .F. ) ;
#13336 = ADVANCED_FACE ( 'NONE', ( #3258 ), #2071, .T. ) ;
#13337 = CARTESIAN_POINT ( 'NONE',  ( -0.5860051159906336515, -0.003937007874015747977, 0.1591122789105256785 ) ) ;
#13338 = DIRECTION ( 'NONE',  ( 0.000000000000000000, 0.000000000000000000, 1.000000000000000000 ) ) ;
#13339 = TOROIDAL_SURFACE ( 'NONE', #3331, 3.149606299212599048, 0.01968503937007873988 ) ;
#13340 = CIRCLE ( 'NONE', #4079, 0.03937007874015761855 ) ;
#13341 = AXIS2_PLACEMENT_3D ( 'NONE', #7762, #13798, #12550 ) ;
#13342 = DIRECTION ( 'NONE',  ( 0.000000000000000000, 0.000000000000000000, -1.000000000000000000 ) ) ;
#13343 = SPHERICAL_SURFACE ( 'NONE', #14843, 0.003937007874015747977 ) ;
#13344 = CIRCLE ( 'NONE', #10329, 0.01968503937007874682 ) ;
#13345 = CARTESIAN_POINT ( 'NONE',  ( -1.267392367206187309, 35.08612325493829331, 0.5953473710235287486 ) ) ;
#13346 = LINE ( 'NONE', #9913, #10118 ) ;
#13347 = CARTESIAN_POINT ( 'NONE',  ( -0.03044903239804773801, 0.1717056406757087039, 0.01152843233334087912 ) ) ;
#13348 = CARTESIAN_POINT ( 'NONE',  ( 1.181102362204724310, 0.1279527559055117225, 0.02952755905511811330 ) ) ;
#13349 = CARTESIAN_POINT ( 'NONE',  ( 0.06692913385832209572, -0.09842519685039370636, -0.2377126739437405434 ) ) ;
#13350 = DIRECTION ( 'NONE',  ( 0.000000000000000000, 1.000000000000000000, 0.000000000000000000 ) ) ;
#13351 = DIRECTION ( 'NONE',  ( -0.8660254037844405950, 0.000000000000000000, -0.4999999999999966693 ) ) ;
#13352 = DIRECTION ( 'NONE',  ( -1.000000000000000000, 1.224646799147296261E-16, 0.000000000000000000 ) ) ;
#13353 = CIRCLE ( 'NONE', #8098, 0.007874015748031449116 ) ;
#13354 = AXIS2_PLACEMENT_3D ( 'NONE', #6911, #5559, #5494 ) ;
#13355 = EDGE_CURVE ( 'NONE', #14974, #4713, #15157, .T. ) ;
#13356 = VERTEX_POINT ( 'NONE', #2474 ) ;
#13357 = AXIS2_PLACEMENT_3D ( 'NONE', #10701, #10835, #995 ) ;
#13358 = VECTOR ( 'NONE', #12565, 39.37007874015748143 ) ;
#13359 = VERTEX_POINT ( 'NONE', #2768 ) ;
#13360 = ADVANCED_FACE ( 'NONE', ( #2536 ), #13913, .T. ) ;
#13361 = CARTESIAN_POINT ( 'NONE',  ( -2.109904669632267193, -1.821353904148520275, -0.1053094779739250780 ) ) ;
#13362 = CARTESIAN_POINT ( 'NONE',  ( -1.181102362204724310, 0.000000000000000000, 0.02559055118110236185 ) ) ;
#13363 = CIRCLE ( 'NONE', #4849, 0.003937007874015724558 ) ;
#13364 = VECTOR ( 'NONE', #9370, 39.37007874015748143 ) ;
#13365 = CARTESIAN_POINT ( 'NONE',  ( 0.2919796512831356883, -0.2952755905511811330, 0.2458576371656085724 ) ) ;
#13366 = AXIS2_PLACEMENT_3D ( 'NONE', #6973, #4703, #11763 ) ;
#13367 = ADVANCED_FACE ( 'NONE', ( #10924 ), #1296, .T. ) ;
#13368 = DIRECTION ( 'NONE',  ( 0.000000000000000000, 0.000000000000000000, 1.000000000000000000 ) ) ;
#13369 = AXIS2_PLACEMENT_3D ( 'NONE', #6549, #711, #7980 ) ;
#13370 = DIRECTION ( 'NONE',  ( -1.000000000000000000, 0.000000000000000000, 0.000000000000000000 ) ) ;
#13371 = DIRECTION ( 'NONE',  ( 0.000000000000000000, 0.000000000000000000, -1.000000000000000000 ) ) ;
#13372 = ORIENTED_EDGE ( 'NONE', *, *, #1148, .T. ) ;
#13373 = DIRECTION ( 'NONE',  ( 0.000000000000000000, -0.000000000000000000, -1.000000000000000000 ) ) ;
#13374 = FACE_OUTER_BOUND ( 'NONE', #1303, .T. ) ;
#13375 = DIRECTION ( 'NONE',  ( 0.000000000000000000, 1.000000000000000000, 0.000000000000000000 ) ) ;
#13376 = VERTEX_POINT ( 'NONE', #5112 ) ;
#13377 = VERTEX_POINT ( 'NONE', #11064 ) ;
#13378 = CIRCLE ( 'NONE', #865, 0.007874015748031499423 ) ;
#13379 = VERTEX_POINT ( 'NONE', #14696 ) ;
#13380 = VECTOR ( 'NONE', #15305, 39.37007874015748143 ) ;
#13381 = CLOSED_SHELL ( 'NONE', ( #13360, #2944, #10232, #3676, #12832, #12697, #10083, #5573, #11846, #12300, #7987, #12086, #10119, #9434, #1272, #4773, #6435, #11410, #4714, #6047, #13933, #1755, #5173, #2507, #8003, #11486, #13082, #9211, #526 ) ) ;
#13382 = ORIENTED_EDGE ( 'NONE', *, *, #8579, .F. ) ;
#13383 =( BOUNDED_SURFACE ( )  B_SPLINE_SURFACE ( 3, 2, ( 
 ( #10911, #109, #2457 ),
 ( #9674, #4874, #13492 ),
 ( #2755, #12315, #10756 ),
 ( #4792, #199, #7234 ),
 ( #3712, #8487, #4956 ),
 ( #9751, #14520, #14757 ),
 ( #6658, #8787, #8960 ),
 ( #4013, #6499, #6569 ),
 ( #11367, #7760, #1808 ),
 ( #6339, #2821, #3146 ) ),
 .UNSPECIFIED., .F., .F., .T. ) 
 B_SPLINE_SURFACE_WITH_KNOTS ( ( 4, 2, 2, 2, 4 ),
 ( 3, 3 ),
 ( 0.004862229905983068978, 0.005359824983622663366, 0.005857420061262256887, 0.006355015138901850408, 0.006852610216541444796 ),
 ( 0.000000000000000000, 1.000000000000000000 ),
 .UNSPECIFIED. ) 
 GEOMETRIC_REPRESENTATION_ITEM ( )  RATIONAL_B_SPLINE_SURFACE ( (
 ( 1.000000000000000000, 0.7071067811865475727, 1.000000000000000000),
 ( 1.000000000000000000, 0.7118664854617688942, 1.000000000000000000),
 ( 1.000000000000000000, 0.7168001159655631449, 1.000000000000000000),
 ( 1.000000000000000000, 0.7268793899691540217, 1.000000000000000000),
 ( 1.000000000000000000, 0.7317766985259492873, 1.000000000000000000),
 ( 1.000000000000000000, 0.7409494124080542310, 1.000000000000000000),
 ( 1.000000000000000000, 0.7450318297967697401, 1.000000000000000000),
 ( 1.000000000000000000, 0.7517743552594693401, 1.000000000000000000),
 ( 1.000000000000000000, 0.7543262850462577607, 1.000000000000000000),
 ( 1.000000000000000000, 0.7558617697692807669, 1.000000000000000000) ) ) 
 REPRESENTATION_ITEM ( '' )  SURFACE ( )  );
#13384 = ORIENTED_EDGE ( 'NONE', *, *, #12836, .F. ) ;
#13385 = AXIS2_PLACEMENT_3D ( 'NONE', #5305, #5540, #1802 ) ;
#13386 = DIRECTION ( 'NONE',  ( -0.000000000000000000, -1.000000000000000000, -0.000000000000000000 ) ) ;
#13387 = FACE_OUTER_BOUND ( 'NONE', #221, .T. ) ;
#13388 = FACE_OUTER_BOUND ( 'NONE', #11158, .T. ) ;
#13389 = EDGE_CURVE ( 'NONE', #6409, #11475, #5389, .T. ) ;
#13390 = CARTESIAN_POINT ( 'NONE',  ( -0.07635964791965738074, -0.1878198040935885327, -0.03937007874015747977 ) ) ;
#13391 = CARTESIAN_POINT ( 'NONE',  ( -2.188516668593762038, -1.823600774915123957, 0.1033333524257560032 ) ) ;
#13392 = AXIS2_PLACEMENT_3D ( 'NONE', #7522, #7755, #327 ) ;
#13393 = CARTESIAN_POINT ( 'NONE',  ( -1.115439883890946726, -0.06270839865334709717, 0.03937007874015747977 ) ) ;
#13394 = CARTESIAN_POINT ( 'NONE',  ( -1.886696118240337450, -2.905094481821793639, 0.07206890175680845390 ) ) ;
#13395 = CIRCLE ( 'NONE', #14395, 0.04330708661417331101 ) ;
#13396 = ORIENTED_EDGE ( 'NONE', *, *, #8162, .F. ) ;
#13397 = CARTESIAN_POINT ( 'NONE',  ( -1.969094085985442444, -2.872830032507542874, 0.1272935473072890067 ) ) ;
#13398 = CARTESIAN_POINT ( 'NONE',  ( -0.5905511811023621549, 2.440944881889763884, 0.000000000000000000 ) ) ;
#13399 = AXIS2_PLACEMENT_3D ( 'NONE', #5060, #2658, #1490 ) ;
#13400 = DIRECTION ( 'NONE',  ( -0.8660254037844363761, -4.956352788505160310E-16, 0.5000000000000041078 ) ) ;
#13401 = ORIENTED_EDGE ( 'NONE', *, *, #1352, .F. ) ;
#13402 = ORIENTED_EDGE ( 'NONE', *, *, #5667, .F. ) ;
#13404 = ORIENTED_EDGE ( 'NONE', *, *, #11823, .T. ) ;
#13403 = CIRCLE ( 'NONE', #10151, 0.04330708661417331101 ) ;
#13405 = LINE ( 'NONE', #11514, #6346 ) ;
#13406 = CIRCLE ( 'NONE', #7902, 0.01968503937007880233 ) ;
#13407 =( REPRESENTATION_RELATIONSHIP ('NONE','NONE', #8904, #2403 ) REPRESENTATION_RELATIONSHIP_WITH_TRANSFORMATION ( #11706 )SHAPE_REPRESENTATION_RELATIONSHIP( ) );
#13408 = DIRECTION ( 'NONE',  ( 4.292327424963333000E-16, 1.000000000000000000, 2.478176394252540219E-16 ) ) ;
#13409 = DIRECTION ( 'NONE',  ( -0.000000000000000000, 1.000000000000000000, -0.000000000000000000 ) ) ;
#13410 = CARTESIAN_POINT ( 'NONE',  ( -0.1181102362204724809, 2.440944881889763884, 0.04724409448818898266 ) ) ;
#13411 = CARTESIAN_POINT ( 'NONE',  ( -0.02220179245438161017, -0.1805881202044197775, -0.03580963740886420471 ) ) ;
#13412 = EDGE_LOOP ( 'NONE', ( #3015, #5975, #4476, #2827, #9944, #5990, #9795, #7909, #7266, #9278, #10165, #958, #13480, #14642, #7020, #14392 ) ) ;
#13413 = FACE_OUTER_BOUND ( 'NONE', #5534, .T. ) ;
#13414 = CARTESIAN_POINT ( 'NONE',  ( -0.06692913385815735250, -0.4921259842519685179, -0.5870514566507987197 ) ) ;
#13415 = CARTESIAN_POINT ( 'NONE',  ( -0.06299212598414173636, -0.4921259842519685179, -0.2366577558633980449 ) ) ;
#13416 = MECHANICAL_DESIGN_GEOMETRIC_PRESENTATION_REPRESENTATION (  '', ( #921 ), #6644 ) ;
#13417 = DIRECTION ( 'NONE',  ( 0.000000000000000000, 1.000000000000000000, 0.000000000000000000 ) ) ;
#13418 = EDGE_CURVE ( 'NONE', #13771, #4031, #2650, .T. ) ;
#13419 = CARTESIAN_POINT ( 'NONE',  ( 0.000000000000000000, 0.3228346456692913757, 0.000000000000000000 ) ) ;
#13420 = VECTOR ( 'NONE', #4872, 39.37007874015748854 ) ;
#13421 = VERTEX_POINT ( 'NONE', #9917 ) ;
#13422 = ORIENTED_EDGE ( 'NONE', *, *, #4833, .F. ) ;
#13423 = ORIENTED_EDGE ( 'NONE', *, *, #7677, .T. ) ;
#13424 = ORIENTED_EDGE ( 'NONE', *, *, #8292, .F. ) ;
#13425 = DIRECTION ( 'NONE',  ( 1.000000000000000000, 0.000000000000000000, 0.000000000000000000 ) ) ;
#13426 = CARTESIAN_POINT ( 'NONE',  ( -0.06692913385815747740, -0.4881889763779528324, -0.2377126739438355507 ) ) ;
#13427 = CARTESIAN_POINT ( 'NONE',  ( -1.974289017530427071, -2.655922424065692677, 0.1447746667326335335 ) ) ;
#13428 = DIRECTION ( 'NONE',  ( -0.000000000000000000, 0.000000000000000000, 1.000000000000000000 ) ) ;
#13429 = DIRECTION ( 'NONE',  ( 0.4333736175764352772, 0.8657846595920661859, 0.2502083747674396785 ) ) ;
#13430 = DIRECTION ( 'NONE',  ( 0.4999999999999999445, 0.000000000000000000, 0.8660254037844387076 ) ) ;
#13431 = AXIS2_PLACEMENT_3D ( 'NONE', #1437, #9813, #14581 ) ;
#13432 = EDGE_CURVE ( 'NONE', #6371, #6490, #6639, .T. ) ;
#13433 = LINE ( 'NONE', #12103, #8858 ) ;
#13434 = DIRECTION ( 'NONE',  ( 1.000000000000000000, -0.000000000000000000, 1.224646799147353207E-16 ) ) ;
#13435 = CARTESIAN_POINT ( 'NONE',  ( 0.000000000000000000, 1.385826771653543510, 0.000000000000000000 ) ) ;
#13436 = CIRCLE ( 'NONE', #11697, 0.003937007874015758385 ) ;
#13437 = DIRECTION ( 'NONE',  ( 0.08093398607328358696, 0.9967194639908912857, 1.383226122518417559E-14 ) ) ;
#13438 = ADVANCED_FACE ( 'NONE', ( #6211 ), #2394, .T. ) ;
#13439 = PLANE ( 'NONE',  #4914 ) ;
#13440 = AXIS2_PLACEMENT_3D ( 'NONE', #13140, #1393, #14714 ) ;
#13441 = VERTEX_POINT ( 'NONE', #10838 ) ;
#13442 = ORIENTED_EDGE ( 'NONE', *, *, #988, .T. ) ;
#13443 = CIRCLE ( 'NONE', #5925, 0.01968503937007873988 ) ;
#13444 = VERTEX_POINT ( 'NONE', #11001 ) ;
#13445 = PRODUCT_DEFINITION_SHAPE ( 'NONE', 'NONE',  #15489 ) ;
#13446 = EDGE_CURVE ( 'NONE', #8855, #9877, #4806, .T. ) ;
#13447 = DIRECTION ( 'NONE',  ( 0.000000000000000000, 0.000000000000000000, 1.000000000000000000 ) ) ;
#13448 = CARTESIAN_POINT ( 'NONE',  ( -1.929243765392412602, -2.937949247912258866, 0.06324214348988090040 ) ) ;
#13449 = DIRECTION ( 'NONE',  ( 0.000000000000000000, 0.000000000000000000, 1.000000000000000000 ) ) ;
#13450 = ADVANCED_FACE ( 'NONE', ( #127 ), #3956, .T. ) ;
#13451 = DIRECTION ( 'NONE',  ( -0.6722799013647310362, 0.7402970580929166822, 0.000000000000000000 ) ) ;
#13452 = CARTESIAN_POINT ( 'NONE',  ( -1.979000582895977356, -2.792299510989483924, -0.1761417809285775182 ) ) ;
#13453 =( GEOMETRIC_REPRESENTATION_CONTEXT ( 3 ) GLOBAL_UNCERTAINTY_ASSIGNED_CONTEXT ( ( #10189 ) ) GLOBAL_UNIT_ASSIGNED_CONTEXT ( ( #13101, #15153, #4493 ) ) REPRESENTATION_CONTEXT ( 'NONE', 'WORKASPACE' ) );
#13454 = DIRECTION ( 'NONE',  ( -0.000000000000000000, -1.000000000000000000, -0.000000000000000000 ) ) ;
#13455 = CARTESIAN_POINT ( 'NONE',  ( -1.883869515785526749, -2.912065805618242909, 0.05637122295548225442 ) ) ;
#13456 = EDGE_CURVE ( 'NONE', #1832, #13926, #9767, .T. ) ;
#13457 = DIRECTION ( 'NONE',  ( 0.000000000000000000, 0.000000000000000000, 1.000000000000000000 ) ) ;
#13458 = FACE_OUTER_BOUND ( 'NONE', #2158, .T. ) ;
#13459 = ORIENTED_EDGE ( 'NONE', *, *, #424, .F. ) ;
#13460 = ORIENTED_EDGE ( 'NONE', *, *, #7552, .T. ) ;
#13461 = CIRCLE ( 'NONE', #6691, 0.003937007874015724558 ) ;
#13462 = ORIENTED_EDGE ( 'NONE', *, *, #13276, .T. ) ;
#13463 = VERTEX_POINT ( 'NONE', #9828 ) ;
#13464 = ORIENTED_EDGE ( 'NONE', *, *, #1760, .T. ) ;
#13465 = CIRCLE ( 'NONE', #14730, 0.1574803149606299191 ) ;
#13466 = CARTESIAN_POINT ( 'NONE',  ( 0.000000000000000000, 0.07874015748031495954, 0.000000000000000000 ) ) ;
#13467 = CYLINDRICAL_SURFACE ( 'NONE', #8917, 0.003937007874015721089 ) ;
#13468 = CARTESIAN_POINT ( 'NONE',  ( 0.05905511811023622659, 1.190944881889763884, -0.8267716535433072833 ) ) ;
#13469 = DIRECTION ( 'NONE',  ( 0.3150766955165275607, -0.9411644975924604584, 0.1222131924708509537 ) ) ;
#13470 = CARTESIAN_POINT ( 'NONE',  ( -2.168819294502306594, -1.823050691322464223, 0.1033464566929130080 ) ) ;
#13472 = CIRCLE ( 'NONE', #1958, 0.5590551181102362266 ) ;
#13471 = SPHERICAL_SURFACE ( 'NONE', #13229, 0.003937007874015747977 ) ;
#13473 = CARTESIAN_POINT ( 'NONE',  ( -1.882336498508431433, -2.915825039791433149, -0.04527253493000575613 ) ) ;
#13474 = ORIENTED_EDGE ( 'NONE', *, *, #5306, .F. ) ;
#13475 = DIRECTION ( 'NONE',  ( -1.000000000000000000, -0.000000000000000000, -0.000000000000000000 ) ) ;
#13476 = CARTESIAN_POINT ( 'NONE',  ( -1.590143285779367810, 0.1215581459421218452, 0.06156531251089462919 ) ) ;
#13477 = EDGE_CURVE ( 'NONE', #2079, #2454, #12677, .T. ) ;
#13478 = CARTESIAN_POINT ( 'NONE',  ( -1.398125690441303304, -0.003404927804347070153, -0.05905511811023622659 ) ) ;
#13479 = EDGE_LOOP ( 'NONE', ( #10693, #3549, #5915, #8507 ) ) ;
#13480 = ORIENTED_EDGE ( 'NONE', *, *, #2648, .T. ) ;
#13481 = EDGE_CURVE ( 'NONE', #9857, #13695, #3794, .T. ) ;
#13482 = EDGE_CURVE ( 'NONE', #1905, #7883, #14608, .T. ) ;
#13483 = ORIENTED_EDGE ( 'NONE', *, *, #9029, .F. ) ;
#13484 = CARTESIAN_POINT ( 'NONE',  ( -0.5860051159906336515, -0.09448818897637796532, 0.1591122789105256785 ) ) ;
#13485 = CARTESIAN_POINT ( 'NONE',  ( -1.181102362204724310, 0.000000000000000000, 0.02952755905511811330 ) ) ;
#13486 = CARTESIAN_POINT ( 'NONE',  ( -1.387704745771440207, -0.02010536753476144939, -0.03937007874015747977 ) ) ;
#13487 = DIRECTION ( 'NONE',  ( -1.000000000000000000, -0.000000000000000000, -1.445602896647339903E-16 ) ) ;
#13488 = CARTESIAN_POINT ( 'NONE',  ( -0.007502606504445012009, -0.1783918715466182581, -0.01493773385587683807 ) ) ;
#13489 = ORIENTED_EDGE ( 'NONE', *, *, #1188, .T. ) ;
#13490 = CARTESIAN_POINT ( 'NONE',  ( -2.090051324975654268, -1.858423098537180129, 0.08664193191037310171 ) ) ;
#13491 = CARTESIAN_POINT ( 'NONE',  ( -0.05905511811012585655, -0.1023622047244094474, -0.5870514566507987197 ) ) ;
#13492 = CARTESIAN_POINT ( 'NONE',  ( -0.06997480235680504645, -0.1674783595965826377, 0.05905511811023622659 ) ) ;
#13493 = ORIENTED_EDGE ( 'NONE', *, *, #11662, .T. ) ;
#13494 = ORIENTED_EDGE ( 'NONE', *, *, #13784, .F. ) ;
#13495 = DIRECTION ( 'NONE',  ( -0.000000000000000000, -0.000000000000000000, -1.000000000000000000 ) ) ;
#13496 = CARTESIAN_POINT ( 'NONE',  ( 0.1259842519685039353, 2.440944881889763884, -0.04724409448818898266 ) ) ;
#13497 = CARTESIAN_POINT ( 'NONE',  ( -1.979215166314494567, -2.704546138957998114, 0.1698509068488507356 ) ) ;
#13498 = DIRECTION ( 'NONE',  ( 1.000000000000000000, 0.000000000000000000, 0.000000000000000000 ) ) ;
#13499 = PRODUCT_CONTEXT ( 'NONE', #3510, 'mechanical' ) ;
#13500 = CARTESIAN_POINT ( 'NONE',  ( -1.416802626423024680, -0.01064955486146301061, 0.06801238946443101396 ) ) ;
#13501 = DIRECTION ( 'NONE',  ( -0.000000000000000000, -0.000000000000000000, 1.000000000000000000 ) ) ;
#13502 = DIRECTION ( 'NONE',  ( -1.000000000000000000, 0.000000000000000000, 0.000000000000000000 ) ) ;
#13503 = DIRECTION ( 'NONE',  ( 0.000000000000000000, 0.000000000000000000, -1.000000000000000000 ) ) ;
#13504 = DIRECTION ( 'NONE',  ( 1.445602896647339903E-16, 0.000000000000000000, -1.000000000000000000 ) ) ;
#13505 = CARTESIAN_POINT ( 'NONE',  ( 7.232166136696967594E-17, 0.000000000000000000, 0.5905511811023621549 ) ) ;
#13506 = ORIENTED_EDGE ( 'NONE', *, *, #6763, .T. ) ;
#13507 = VERTEX_POINT ( 'NONE', #7396 ) ;
#13508 = EDGE_CURVE ( 'NONE', #9167, #8519, #3665, .T. ) ;
#13509 = VERTEX_POINT ( 'NONE', #1523 ) ;
#13510 = EDGE_CURVE ( 'NONE', #3814, #113, #11476, .T. ) ;
#13511 = ORIENTED_EDGE ( 'NONE', *, *, #11828, .F. ) ;
#13512 = EDGE_CURVE ( 'NONE', #2402, #12118, #4023, .T. ) ;
#13513 = DIRECTION ( 'NONE',  ( -0.000000000000000000, 1.000000000000000000, 0.000000000000000000 ) ) ;
#13514 = CARTESIAN_POINT ( 'NONE',  ( -1.930132312531408934, -2.935508558968578097, 0.06929162352469166175 ) ) ;
#13515 = DIRECTION ( 'NONE',  ( -1.000000000000000000, 0.000000000000000000, 0.000000000000000000 ) ) ;
#13516 = CARTESIAN_POINT ( 'NONE',  ( -1.180847381051866485, 0.3433074774306730248, -0.04457070858981632827 ) ) ;
#13517 = DIRECTION ( 'NONE',  ( 1.000000000000000000, 0.000000000000000000, 0.000000000000000000 ) ) ;
#13518 = FACE_OUTER_BOUND ( 'NONE', #9855, .T. ) ;
#13519 = CARTESIAN_POINT ( 'NONE',  ( 0.9851651268172137987, -1.725292181286280480, -0.08366141732283420562 ) ) ;
#13520 = CARTESIAN_POINT ( 'NONE',  ( -1.919180121628701441, -2.820811045952824170, -0.1478741305074587342 ) ) ;
#13521 = LINE ( 'NONE', #8449, #2563 ) ;
#13522 = CARTESIAN_POINT ( 'NONE',  ( 0.4841913566216283216, 1.338782396965247257, 0.3477389867607208473 ) ) ;
#13523 = ORIENTED_EDGE ( 'NONE', *, *, #1214, .T. ) ;
#13524 = EDGE_CURVE ( 'NONE', #9980, #8323, #11229, .T. ) ;
#13525 = EDGE_LOOP ( 'NONE', ( #14984, #6000, #8533, #13560, #15197, #2294 ) ) ;
#13526 = ORIENTED_EDGE ( 'NONE', *, *, #4674, .T. ) ;
#13527 = ADVANCED_FACE ( 'NONE', ( #13748 ), #10416, .T. ) ;
#13528 = ORIENTED_EDGE ( 'NONE', *, *, #6509, .T. ) ;
#13529 = VERTEX_POINT ( 'NONE', #11153 ) ;
#13530 = CARTESIAN_POINT ( 'NONE',  ( -1.395815242326012617, -0.02537006130049591218, -0.04028299403797801215 ) ) ;
#13531 = EDGE_CURVE ( 'NONE', #8021, #9271, #1822, .T. ) ;
#13532 = EDGE_CURVE ( 'NONE', #12009, #10253, #1178, .T. ) ;
#13533 = DIRECTION ( 'NONE',  ( -1.000000000000000000, 0.000000000000000000, 0.000000000000000000 ) ) ;
#13534 = FACE_BOUND ( 'NONE', #6474, .T. ) ;
#13535 = DIRECTION ( 'NONE',  ( 1.224646799147352961E-16, 0.000000000000000000, -1.000000000000000000 ) ) ;
#13536 = DIRECTION ( 'NONE',  ( -1.224646799147352961E-16, 0.000000000000000000, -1.000000000000000000 ) ) ;
#13537 = CARTESIAN_POINT ( 'NONE',  ( -1.872041180245539449, -2.941023256354079241, 0.05466348536124700924 ) ) ;
#13538 = ORIENTED_EDGE ( 'NONE', *, *, #404, .T. ) ;
#13539 = FACE_OUTER_BOUND ( 'NONE', #11290, .T. ) ;
#13540 = CARTESIAN_POINT ( 'NONE',  ( -1.584115185264708847, 0.1296286773226380806, 0.05905511811023622659 ) ) ;
#13541 = CARTESIAN_POINT ( 'NONE',  ( 0.000000000000000000, 1.370078740157480546, 0.000000000000000000 ) ) ;
#13542 = ORIENTED_EDGE ( 'NONE', *, *, #10893, .F. ) ;
#13543 = ORIENTED_EDGE ( 'NONE', *, *, #1233, .F. ) ;
#13544 = VERTEX_POINT ( 'NONE', #11235 ) ;
#13545 = ADVANCED_FACE ( 'NONE', ( #1685 ), #12564, .F. ) ;
#13546 = ADVANCED_FACE ( 'NONE', ( #6676 ), #2905, .T. ) ;
#13547 = DIRECTION ( 'NONE',  ( -0.8660254037844432595, 0.000000000000000000, -0.4999999999999918954 ) ) ;
#13548 = DIRECTION ( 'NONE',  ( -0.5801894994542512451, -0.8144815189573213488, 0.000000000000000000 ) ) ;
#13549 = DIRECTION ( 'NONE',  ( 0.4999999999999966693, 0.000000000000000000, 0.8660254037844405950 ) ) ;
#13550 = CARTESIAN_POINT ( 'NONE',  ( -0.002197004598026061628, -0.1775723205537574900, 0.001204381035045432730 ) ) ;
#13551 = VERTEX_POINT ( 'NONE', #8975 ) ;
#13552 = DIRECTION ( 'NONE',  ( 0.4999999999999920064, 0.000000000000000000, -0.8660254037844433705 ) ) ;
#13553 = EDGE_CURVE ( 'NONE', #12443, #5050, #913, .T. ) ;
#13554 = CARTESIAN_POINT ( 'NONE',  ( 0.4751993499420012479, 1.346456692913385877, 0.3506226965216235336 ) ) ;
#13555 = CARTESIAN_POINT ( 'NONE',  ( -0.4841913566216236031, 1.338782396965247257, 0.3477389867607276752 ) ) ;
#13556 = PRODUCT_DEFINITION_SHAPE ( 'NONE', 'NONE',  #15477 ) ;
#13557 = CARTESIAN_POINT ( 'NONE',  ( -0.1062992125983150127, -0.4921259842519685179, -0.2482618547482104143 ) ) ;
#13558 = VERTEX_POINT ( 'NONE', #9041 ) ;
#13559 = VERTEX_POINT ( 'NONE', #4097 ) ;
#13560 = ORIENTED_EDGE ( 'NONE', *, *, #4194, .F. ) ;
#13561 = DIRECTION ( 'NONE',  ( -1.000000000000000000, 0.000000000000000000, 0.000000000000000000 ) ) ;
#13562 = CARTESIAN_POINT ( 'NONE',  ( 0.3137366569588399545, -0.2952755905511811330, 0.2947875711430715251 ) ) ;
#13563 = CARTESIAN_POINT ( 'NONE',  ( -1.999703161025048193, -2.564938650654521091, 0.1343432867203113723 ) ) ;
#13564 = CYLINDRICAL_SURFACE ( 'NONE', #11366, 0.03937007874015751446 ) ;
#13565 = DIRECTION ( 'NONE',  ( 1.000000000000000000, 0.000000000000000000, 0.000000000000000000 ) ) ;
#13566 = LINE ( 'NONE', #10051, #6580 ) ;
#13567 = DIRECTION ( 'NONE',  ( 1.000000000000000000, 0.000000000000000000, 0.000000000000000000 ) ) ;
#13568 = DIRECTION ( 'NONE',  ( 0.8660254037844368202, 0.000000000000000000, -0.5000000000000032196 ) ) ;
#13569 = ADVANCED_FACE ( 'NONE', ( #5188 ), #12647, .F. ) ;
#13570 = CARTESIAN_POINT ( 'NONE',  ( 1.309055118110236116, 4.044111181948214319E-16, -0.02559055118110236185 ) ) ;
#13571 = DIRECTION ( 'NONE',  ( 0.000000000000000000, 0.000000000000000000, 1.000000000000000000 ) ) ;
#13572 = DIRECTION ( 'NONE',  ( 0.8660254037844347108, 0.000000000000000000, -0.5000000000000069944 ) ) ;
#13573 = ORIENTED_EDGE ( 'NONE', *, *, #4679, .F. ) ;
#13574 = ORIENTED_EDGE ( 'NONE', *, *, #8883, .F. ) ;
#13576 = ORIENTED_EDGE ( 'NONE', *, *, #546, .T. ) ;
#13575 = CIRCLE ( 'NONE', #12333, 0.5984251968503937480 ) ;
#13577 = VECTOR ( 'NONE', #8813, 39.37007874015748143 ) ;
#13578 = ORIENTED_EDGE ( 'NONE', *, *, #5843, .T. ) ;
#13579 = TOROIDAL_SURFACE ( 'NONE', #14081, 0.04330708661417328326, 0.003937007874015747977 ) ;
#13580 = CIRCLE ( 'NONE', #3079, 0.1574803149606299191 ) ;
#13581 = CARTESIAN_POINT ( 'NONE',  ( -0.2362204724409448231, -0.02638708502139245488, -0.03937007874015747977 ) ) ;
#13582 = CARTESIAN_POINT ( 'NONE',  ( -1.950933367886963365, -2.918556150189103526, -0.1002687663322968242 ) ) ;
#13583 = LINE ( 'NONE', #7644, #9716 ) ;
#13584 = FACE_OUTER_BOUND ( 'NONE', #12856, .T. ) ;
#13585 = DIRECTION ( 'NONE',  ( 0.000000000000000000, 0.000000000000000000, 1.000000000000000000 ) ) ;
#13586 = AXIS2_PLACEMENT_3D ( 'NONE', #8509, #3805, #14620 ) ;
#13587 = AXIS2_PLACEMENT_3D ( 'NONE', #12188, #6127, #4964 ) ;
#13588 = DIRECTION ( 'NONE',  ( 1.000000000000000000, 0.000000000000000000, 3.973232667114495301E-16 ) ) ;
#13589 = EDGE_CURVE ( 'NONE', #12219, #6685, #14425, .T. ) ;
#13590 = CARTESIAN_POINT ( 'NONE',  ( -0.02018259705034725071, -0.1802452534892125813, 1.049219007154695292E-17 ) ) ;
#13591 = AXIS2_PLACEMENT_3D ( 'NONE', #3147, #12851, #2122 ) ;
#13592 = CARTESIAN_POINT ( 'NONE',  ( 0.000000000000000000, 2.637795275590551825, 0.03937007874015747977 ) ) ;
#13593 = CARTESIAN_POINT ( 'NONE',  ( 0.000000000000000000, 1.377952755905512028, 0.5984251968503937480 ) ) ;
#13594 = AXIS2_PLACEMENT_3D ( 'NONE', #6678, #4255, #3078 ) ;
#13595 = ORIENTED_EDGE ( 'NONE', *, *, #8343, .T. ) ;
#13596 = EDGE_CURVE ( 'NONE', #14774, #9212, #3916, .T. ) ;
#13597 = ORIENTED_EDGE ( 'NONE', *, *, #13510, .T. ) ;
#13598 = B_SPLINE_CURVE_WITH_KNOTS ( 'NONE', 3,
 ( #2518, #6191, #1345, #10982, #4951, #11945, #263, #10905 ),
 .UNSPECIFIED., .F., .F.,
 ( 4, 2, 2, 4 ),
 ( 0.000000000000000000, 0.0009271389380264786345, 0.001390708407039718385, 0.001854277876052958136 ),
 .UNSPECIFIED. ) ;
#13599 = ORIENTED_EDGE ( 'NONE', *, *, #3420, .T. ) ;
#13600 = EDGE_LOOP ( 'NONE', ( #9260, #11693, #14087, #6472 ) ) ;
#13601 = ORIENTED_EDGE ( 'NONE', *, *, #6336, .T. ) ;
#13602 = VECTOR ( 'NONE', #14465, 39.37007874015748143 ) ;
#13603 = CIRCLE ( 'NONE', #114, 0.003937007874015750579 ) ;
#13604 = CARTESIAN_POINT ( 'NONE',  ( -1.395764539142011706, -0.02487486760722468909, -0.06610458043051951893 ) ) ;
#13605 = VECTOR ( 'NONE', #7070, 39.37007874015748143 ) ;
#13606 = AXIS2_PLACEMENT_3D ( 'NONE', #9594, #14374, #7012 ) ;
#13607 = CYLINDRICAL_SURFACE ( 'NONE', #5561, 0.003937007874015758385 ) ;
#13608 = AXIS2_PLACEMENT_3D ( 'NONE', #12715, #1975, #4473 ) ;
#13609 = CARTESIAN_POINT ( 'NONE',  ( -1.574484809660000373, 0.1100025355994882770, 0.06175692796175874522 ) ) ;
#13610 = TOROIDAL_SURFACE ( 'NONE', #8867, 0.5984251968503937480, 0.007874015748031495954 ) ;
#13611 = FACE_OUTER_BOUND ( 'NONE', #8923, .T. ) ;
#13612 = VECTOR ( 'NONE', #10800, 39.37007874015748143 ) ;
#13613 = FACE_OUTER_BOUND ( 'NONE', #10966, .T. ) ;
#13614 = DIRECTION ( 'NONE',  ( -0.000000000000000000, -1.000000000000000000, -0.000000000000000000 ) ) ;
#13615 = EDGE_CURVE ( 'NONE', #7004, #14646, #175, .T. ) ;
#13616 = DIRECTION ( 'NONE',  ( 0.000000000000000000, -0.000000000000000000, -1.000000000000000000 ) ) ;
#13617 = CARTESIAN_POINT ( 'NONE',  ( -1.181342415325297157, 0.3435647566447596613, 0.03937007874014957637 ) ) ;
#13618 = CARTESIAN_POINT ( 'NONE',  ( -1.875035009920013040, -2.933829477136298713, -0.07328349893415619931 ) ) ;
#13619 = EDGE_CURVE ( 'NONE', #6005, #14240, #7657, .T. ) ;
#13620 = VERTEX_POINT ( 'NONE', #9990 ) ;
#13621 = CARTESIAN_POINT ( 'NONE',  ( -2.010991777528383206, -2.758467574604078987, -0.1561691687464118738 ) ) ;
#13622 = B_SPLINE_CURVE_WITH_KNOTS ( 'NONE', 3,
 ( #3330, #5818, #15324, #13047 ),
 .UNSPECIFIED., .F., .F.,
 ( 4, 4 ),
 ( 0.02290483811074940299, 0.02857925207800687817 ),
 .UNSPECIFIED. ) ;
#13623 = DIRECTION ( 'NONE',  ( -0.5000000000000069944, -8.673617379884209021E-15, 0.8660254037844347108 ) ) ;
#13624 = CIRCLE ( 'NONE', #12137, 0.5984251968503937480 ) ;
#13625 = CIRCLE ( 'NONE', #6103, 0.003937007874015762722 ) ;
#13626 = CARTESIAN_POINT ( 'NONE',  ( -0.002500327830562678200, 0.1532658568795227105, 0.000000000000000000 ) ) ;
#13627 = AXIS2_PLACEMENT_3D ( 'NONE', #7117, #5939, #12144 ) ;
#13628 = ORIENTED_EDGE ( 'NONE', *, *, #8682, .F. ) ;
#13629 = TOROIDAL_SURFACE ( 'NONE', #12124, 0.04330708661417328326, 0.003937007874015747977 ) ;
#13630 = EDGE_CURVE ( 'NONE', #9261, #5839, #15066, .T. ) ;
#13631 = ORIENTED_EDGE ( 'NONE', *, *, #11812, .F. ) ;
#13632 = AXIS2_PLACEMENT_3D ( 'NONE', #6493, #6559, #13640 ) ;
#13633 = UNCERTAINTY_MEASURE_WITH_UNIT (LENGTH_MEASURE( 1.000000000000000082E-05 ), #7788, 'distance_accuracy_value', 'NONE');
#13634 = EDGE_LOOP ( 'NONE', ( #448, #194, #1383, #13803 ) ) ;
#13635 = AXIS2_PLACEMENT_3D ( 'NONE', #9251, #7917, #4470 ) ;
#13636 = AXIS2_PLACEMENT_3D ( 'NONE', #12959, #14214, #11544 ) ;
#13637 = AXIS2_PLACEMENT_3D ( 'NONE', #10611, #3322, #8265 ) ;
#13638 = EDGE_CURVE ( 'NONE', #10586, #10807, #11673, .T. ) ;
#13639 = CARTESIAN_POINT ( 'NONE',  ( 0.1022864650139100745, 0.000000000000000000, 1.563012696487738457E-17 ) ) ;
#13640 = DIRECTION ( 'NONE',  ( 0.5000000000000226485, 0.000000000000000000, -0.8660254037844253849 ) ) ;
#13641 = CARTESIAN_POINT ( 'NONE',  ( 0.1724006475077543565, -0.4881889763779528324, 0.1768186671464649640 ) ) ;
#13642 = CARTESIAN_POINT ( 'NONE',  ( 0.000000000000000000, 0.3070866141732283561, 0.000000000000000000 ) ) ;
#13643 = AXIS2_PLACEMENT_3D ( 'NONE', #11815, #3205, #2015 ) ;
#13644 = CARTESIAN_POINT ( 'NONE',  ( -1.172017912842092668, 0.3609012623030119493, 0.03937007874015747977 ) ) ;
#13645 = ADVANCED_FACE ( 'NONE', ( #12733 ), #14050, .F. ) ;
#13646 = VERTEX_POINT ( 'NONE', #9441 ) ;
#13647 = CARTESIAN_POINT ( 'NONE',  ( -0.6864776960422502849, 1.338582677165354395, 0.4645290592786118222 ) ) ;
#13648 = DIRECTION ( 'NONE',  ( -0.000000000000000000, -1.000000000000000000, -0.000000000000000000 ) ) ;
#13649 = CARTESIAN_POINT ( 'NONE',  ( -1.407020747027296181, -0.03368500256908527751, -0.04737126204478120384 ) ) ;
#13650 = CARTESIAN_POINT ( 'NONE',  ( -1.959562855619890964, -2.764754912074676607, 0.1771653543307128986 ) ) ;
#13651 = EDGE_CURVE ( 'NONE', #3617, #1942, #2661, .T. ) ;
#13652 = AXIS2_PLACEMENT_3D ( 'NONE', #1, #7192, #3444 ) ;
#13653 = AXIS2_PLACEMENT_3D ( 'NONE', #11948, #5618, #11132 ) ;
#13654 = AXIS2_PLACEMENT_3D ( 'NONE', #15295, #9190, #10589 ) ;
#13655 = ORIENTED_EDGE ( 'NONE', *, *, #14574, .T. ) ;
#13656 = EDGE_LOOP ( 'NONE', ( #10291, #6054, #12079, #11808 ) ) ;
#13657 = AXIS2_PLACEMENT_3D ( 'NONE', #1394, #6153, #13288 ) ;
#13658 = ADVANCED_FACE ( 'NONE', ( #4561 ), #3169, .T. ) ;
#13659 = CYLINDRICAL_SURFACE ( 'NONE', #4397, 0.6692913385826770867 ) ;
#13660 = CARTESIAN_POINT ( 'NONE',  ( -0.6864776960422505070, 1.190944881889763884, 0.4645290592786119332 ) ) ;
#13661 = CARTESIAN_POINT ( 'NONE',  ( -1.945459748359986030, -2.745801194614590823, 0.1561691687464110689 ) ) ;
#13662 =( LENGTH_UNIT ( ) NAMED_UNIT ( * ) SI_UNIT ( $, .METRE. ) );
#13663 = TOROIDAL_SURFACE ( 'NONE', #6142, 0.1653543307086614012, 0.007874015748031495954 ) ;
#13664 = DIRECTION ( 'NONE',  ( -1.000000000000000000, 0.000000000000000000, 0.000000000000000000 ) ) ;
#13665 = VECTOR ( 'NONE', #6228, 39.37007874015748143 ) ;
#13666 = DIRECTION ( 'NONE',  ( 0.8660254037844385966, -0.000000000000000000, 0.5000000000000001110 ) ) ;
#13667 = CIRCLE ( 'NONE', #12375, 0.003937007874015721089 ) ;
#13668 = DIRECTION ( 'NONE',  ( -0.4999999999999928946, -0.000000000000000000, -0.8660254037844428154 ) ) ;
#13669 = DIRECTION ( 'NONE',  ( 0.000000000000000000, 0.000000000000000000, 1.000000000000000000 ) ) ;
#13670 = DIRECTION ( 'NONE',  ( 0.8660254037844385966, 0.000000000000000000, 0.5000000000000000000 ) ) ;
#13671 = CIRCLE ( 'NONE', #2166, 0.01968503937007874682 ) ;
#13672 = CARTESIAN_POINT ( 'NONE',  ( -0.4330708661417336236, -0.09448818897637796532, 0.4279391777402706265 ) ) ;
#13673 = ADVANCED_FACE ( 'NONE', ( #15398 ), #4907, .T. ) ;
#13674 = ORIENTED_EDGE ( 'NONE', *, *, #1570, .F. ) ;
#13675 = ORIENTED_EDGE ( 'NONE', *, *, #5853, .F. ) ;
#13676 = EDGE_LOOP ( 'NONE', ( #2155, #1103, #8454, #14938 ) ) ;
#13677 = PRESENTATION_LAYER_ASSIGNMENT (  '', '', ( #921 ) ) ;
#13678 = EDGE_CURVE ( 'NONE', #9785, #10031, #6823, .T. ) ;
#13679 = ORIENTED_EDGE ( 'NONE', *, *, #10463, .T. ) ;
#13680 = EDGE_CURVE ( 'NONE', #713, #7744, #15432, .T. ) ;
#13681 = CIRCLE ( 'NONE', #13180, 0.03937007874015751446 ) ;
#13682 = LINE ( 'NONE', #8985, #5326 ) ;
#13683 = CARTESIAN_POINT ( 'NONE',  ( -1.591501945092674841, 0.08600752902535289957, -0.1033464566929133410 ) ) ;
#13684 =( NAMED_UNIT ( * ) SI_UNIT ( $, .STERADIAN. ) SOLID_ANGLE_UNIT ( ) );
#13685 = DIRECTION ( 'NONE',  ( 0.000000000000000000, 1.000000000000000000, 0.000000000000000000 ) ) ;
#13686 = CARTESIAN_POINT ( 'NONE',  ( -1.977060571132597255, -2.798357741064777748, -0.1753504618005770066 ) ) ;
#13687 = LINE ( 'NONE', #5445, #11854 ) ;
#13688 = MECHANICAL_DESIGN_GEOMETRIC_PRESENTATION_REPRESENTATION (  '', ( #2928 ), #2181 ) ;
#13689 = CARTESIAN_POINT ( 'NONE',  ( 1.224409448818897461, 4.044111181948214319E-16, 0.02559055118110236185 ) ) ;
#13690 = CARTESIAN_POINT ( 'NONE',  ( -1.895297964913681854, -2.883558765292476345, -0.1043903633197201947 ) ) ;
#13691 = CARTESIAN_POINT ( 'NONE',  ( -1.409916934715107484, -0.04334312390809511029, 0.08366141732283458032 ) ) ;
#13692 = LINE ( 'NONE', #9059, #2161 ) ;
#13693 = VECTOR ( 'NONE', #2741, 39.37007874015748143 ) ;
#13694 = ORIENTED_EDGE ( 'NONE', *, *, #14821, .T. ) ;
#13695 = VERTEX_POINT ( 'NONE', #1135 ) ;
#13696 = CIRCLE ( 'NONE', #4181, 0.003937007874015724558 ) ;
#13697 = ORIENTED_EDGE ( 'NONE', *, *, #10059, .T. ) ;
#13698 = ORIENTED_EDGE ( 'NONE', *, *, #9797, .T. ) ;
#13699 = ORIENTED_EDGE ( 'NONE', *, *, #7087, .F. ) ;
#13700 = CIRCLE ( 'NONE', #2437, 0.003937007874015747977 ) ;
#13701 = FACE_OUTER_BOUND ( 'NONE', #4127, .T. ) ;
#13702 = CARTESIAN_POINT ( 'NONE',  ( 0.5398975377803496567, -0.4881889763779528324, 0.2389729469846946508 ) ) ;
#13703 = DIRECTION ( 'NONE',  ( 0.000000000000000000, 1.000000000000000000, -0.000000000000000000 ) ) ;
#13704 = COLOUR_RGB ( '',0.7921568627450980005, 0.8196078431372548767, 0.9333333333333333481 ) ;
#13705 = DIRECTION ( 'NONE',  ( -0.000000000000000000, -1.000000000000000000, -0.000000000000000000 ) ) ;
#13706 = DIRECTION ( 'NONE',  ( 1.000000000000000000, 0.000000000000000000, 0.000000000000000000 ) ) ;
#13707 = DIRECTION ( 'NONE',  ( 0.000000000000000000, 0.000000000000000000, 1.000000000000000000 ) ) ;
#13708 = CARTESIAN_POINT ( 'NONE',  ( 0.000000000000000000, 1.417322834645669438, -0.5590551181102362266 ) ) ;
#13709 = CARTESIAN_POINT ( 'NONE',  ( -1.398495881576244937, -0.02731002314121834529, -0.07874015748031495954 ) ) ;
#13710 = CARTESIAN_POINT ( 'NONE',  ( -1.879669289221657547, -2.922326730264934724, -0.005526921115518252693 ) ) ;
#13711 = ORIENTED_EDGE ( 'NONE', *, *, #13205, .F. ) ;
#13712 = DIRECTION ( 'NONE',  ( 0.000000000000000000, 2.212657494868377674E-16, -1.000000000000000000 ) ) ;
#13713 = DIRECTION ( 'NONE',  ( 0.000000000000000000, 1.000000000000000000, 0.000000000000000000 ) ) ;
#13714 = AXIS2_PLACEMENT_3D ( 'NONE', #9704, #14479, #11011 ) ;
#13716 = ORIENTED_EDGE ( 'NONE', *, *, #12322, .F. ) ;
#13715 =( REPRESENTATION_RELATIONSHIP ('NONE','NONE', #8904, #11075 ) REPRESENTATION_RELATIONSHIP_WITH_TRANSFORMATION ( #13974 )SHAPE_REPRESENTATION_RELATIONSHIP( ) );
#13717 = ORIENTED_EDGE ( 'NONE', *, *, #1283, .T. ) ;
#13718 = CIRCLE ( 'NONE', #12727, 0.003937007874015741038 ) ;
#13719 = EDGE_CURVE ( 'NONE', #8551, #12353, #5887, .T. ) ;
#13720 = ORIENTED_EDGE ( 'NONE', *, *, #9806, .F. ) ;
#13721 = EDGE_CURVE ( 'NONE', #13899, #9959, #13671, .T. ) ;
#13722 = LINE ( 'NONE', #2983, #8369 ) ;
#13723 = AXIS2_PLACEMENT_3D ( 'NONE', #1568, #2910, #13320 ) ;
#13724 = ADVANCED_FACE ( 'NONE', ( #890 ), #12922, .T. ) ;
#13725 = CARTESIAN_POINT ( 'NONE',  ( -0.5894146648244306119, -0.003937007874015747977, 0.1571437749735178357 ) ) ;
#13726 = DIRECTION ( 'NONE',  ( 1.224646799147343593E-16, 0.000000000000000000, -1.000000000000000000 ) ) ;
#13727 = AXIS2_PLACEMENT_3D ( 'NONE', #1471, #8745, #12120 ) ;
#13728 = CARTESIAN_POINT ( 'NONE',  ( -0.05905511811012585655, -0.09448818897637796532, -0.5870514566507987197 ) ) ;
#13729 = DIRECTION ( 'NONE',  ( 0.000000000000000000, 0.000000000000000000, -1.000000000000000000 ) ) ;
#13730 = ORIENTED_EDGE ( 'NONE', *, *, #6715, .T. ) ;
#13731 = CARTESIAN_POINT ( 'NONE',  ( -0.4822834645669299425, -0.1023622047244094474, 0.3466374647693608591 ) ) ;
#13732 = CARTESIAN_POINT ( 'NONE',  ( 0.06299212598430634080, -0.1023622047244094474, -0.2366577558633030653 ) ) ;
#13733 = DIRECTION ( 'NONE',  ( -0.000000000000000000, -0.000000000000000000, -1.000000000000000000 ) ) ;
#13734 = DIRECTION ( 'NONE',  ( -1.000000000000000000, 0.000000000000000000, 0.000000000000000000 ) ) ;
#13735 = DIRECTION ( 'NONE',  ( -0.000000000000000000, -1.000000000000000000, 0.000000000000000000 ) ) ;
#13736 = ORIENTED_EDGE ( 'NONE', *, *, #2467, .T. ) ;
#13737 = EDGE_CURVE ( 'NONE', #13376, #15395, #10587, .T. ) ;
#13738 = VERTEX_POINT ( 'NONE', #8182 ) ;
#13739 = EDGE_CURVE ( 'NONE', #9753, #1180, #6391, .T. ) ;
#13740 = DIRECTION ( 'NONE',  ( 0.000000000000000000, 2.212657494868377674E-16, 1.000000000000000000 ) ) ;
#13741 = LINE ( 'NONE', #4018, #2401 ) ;
#13742 = ADVANCED_FACE ( 'NONE', ( #12958 ), #6997, .F. ) ;
#13743 = DIRECTION ( 'NONE',  ( -0.5000000000000001110, 0.000000000000000000, 0.8660254037844384856 ) ) ;
#13744 = DIRECTION ( 'NONE',  ( 0.4999999999999991118, -2.275781674304493770E-14, 0.8660254037844391517 ) ) ;
#13745 = SHAPE_DEFINITION_REPRESENTATION ( #775, #7785 ) ;
#13746 = FACE_OUTER_BOUND ( 'NONE', #5037, .T. ) ;
#13747 = DIRECTION ( 'NONE',  ( 4.336808689942014285E-16, 0.000000000000000000, -1.000000000000000000 ) ) ;
#13748 = FACE_OUTER_BOUND ( 'NONE', #11711, .T. ) ;
#13749 = CARTESIAN_POINT ( 'NONE',  ( 0.000000000000000000, 0.05114323250695475970, 0.000000000000000000 ) ) ;
#13750 = DIRECTION ( 'NONE',  ( 1.000000000000000000, 0.000000000000000000, 0.000000000000000000 ) ) ;
#13751 = FACE_OUTER_BOUND ( 'NONE', #11141, .T. ) ;
#13752 = ORIENTED_EDGE ( 'NONE', *, *, #10865, .F. ) ;
#13753 = ORIENTED_EDGE ( 'NONE', *, *, #12090, .F. ) ;
#13754 = DIRECTION ( 'NONE',  ( -3.476578583725179813E-16, -0.000000000000000000, 1.000000000000000000 ) ) ;
#13755 = EDGE_LOOP ( 'NONE', ( #177, #3907, #13494, #1564 ) ) ;
#13756 = EDGE_LOOP ( 'NONE', ( #8642, #2142, #14686 ) ) ;
#13757 = DIRECTION ( 'NONE',  ( 0.8144815189573203495, -0.5801894994542524664, 0.000000000000000000 ) ) ;
#13758 = CARTESIAN_POINT ( 'NONE',  ( -1.977712674129580073, -2.850429627681845268, 0.1595853951502894108 ) ) ;
#13759 = ADVANCED_FACE ( 'NONE', ( #11713 ), #808, .F. ) ;
#13760 = CARTESIAN_POINT ( 'NONE',  ( -1.190198933766853706, 0.3259758027579612860, -0.05905511811023622659 ) ) ;
#13761 = CARTESIAN_POINT ( 'NONE',  ( -0.1804058482824386078, -0.4921259842519685179, -0.1041573650692488584 ) ) ;
#13762 = CARTESIAN_POINT ( 'NONE',  ( 0.000000000000000000, 0.000000000000000000, 0.000000000000000000 ) ) ;
#13763 = DIRECTION ( 'NONE',  ( -0.5000000000000001110, 0.000000000000000000, -0.8660254037844384856 ) ) ;
#13764 = EDGE_CURVE ( 'NONE', #7635, #749, #8170, .T. ) ;
#13765 = CYLINDRICAL_SURFACE ( 'NONE', #8330, 0.01968503937007871907 ) ;
#13766 = CARTESIAN_POINT ( 'NONE',  ( -2.005376571220952364, -2.566823862150081847, -0.1327647275340299027 ) ) ;
#13767 = EDGE_LOOP ( 'NONE', ( #11961, #15241, #9401, #9582 ) ) ;
#13768 = EDGE_LOOP ( 'NONE', ( #13599, #6421, #15329, #13322 ) ) ;
#13769 = ORIENTED_EDGE ( 'NONE', *, *, #7721, .F. ) ;
#13770 = ORIENTED_EDGE ( 'NONE', *, *, #4642, .F. ) ;
#13771 = VERTEX_POINT ( 'NONE', #13028 ) ;
#13772 = CARTESIAN_POINT ( 'NONE',  ( 0.000000000000000000, 1.661417322834646049, -0.5905511811023621549 ) ) ;
#13773 = B_SPLINE_CURVE_WITH_KNOTS ( 'NONE', 3,
 ( #5765, #4527, #14176, #2260 ),
 .UNSPECIFIED., .F., .F.,
 ( 4, 4 ),
 ( 0.0009905856238791982925, 0.002309601750613628646 ),
 .UNSPECIFIED. ) ;
#13774 = CARTESIAN_POINT ( 'NONE',  ( 1.181102362204724310, -0.1279527559055113062, 0.02952755905511811330 ) ) ;
#13775 = DIRECTION ( 'NONE',  ( -0.8660254037844501429, 0.000000000000000000, 0.4999999999999798495 ) ) ;
#13776 = DIRECTION ( 'NONE',  ( 0.000000000000000000, -0.000000000000000000, 1.000000000000000000 ) ) ;
#13777 = CARTESIAN_POINT ( 'NONE',  ( -0.1724006475077544398, -0.1023622047244094474, 0.1768186671464649640 ) ) ;
#13778 = FACE_OUTER_BOUND ( 'NONE', #13756, .T. ) ;
#13779 = CARTESIAN_POINT ( 'NONE',  ( 0.5905511811023622659, -0.2952755905511811330, -0.4190977005962939206 ) ) ;
#13780 = CARTESIAN_POINT ( 'NONE',  ( 0.000000000000000000, 0.007874015748031480341, -0.1574803149606299191 ) ) ;
#13781 = CARTESIAN_POINT ( 'NONE',  ( -1.892078352146237652, -2.891862086400596166, -0.1315695375898782160 ) ) ;
#13782 = EDGE_LOOP ( 'NONE', ( #5751, #14289, #6097, #6535 ) ) ;
#13783 = CARTESIAN_POINT ( 'NONE',  ( -2.119211488178678771, -2.391206066312333345, -0.1145569965096258497 ) ) ;
#13784 = EDGE_CURVE ( 'NONE', #10400, #1599, #673, .T. ) ;
#13785 = LINE ( 'NONE', #12536, #4855 ) ;
#13786 = ORIENTED_EDGE ( 'NONE', *, *, #11312, .F. ) ;
#13787 = ORIENTED_EDGE ( 'NONE', *, *, #2702, .T. ) ;
#13788 = ORIENTED_EDGE ( 'NONE', *, *, #11535, .T. ) ;
#13789 = CARTESIAN_POINT ( 'NONE',  ( 0.000000000000000000, 2.161417322834645827, 0.1535433070866141780 ) ) ;
#13790 = CARTESIAN_POINT ( 'NONE',  ( 0.000000000000000000, 0.5590551181102362266, 0.000000000000000000 ) ) ;
#13791 = CARTESIAN_POINT ( 'NONE',  ( 0.000000000000000000, -1.707404996040164512E-17, 0.5826771653543306728 ) ) ;
#13792 = CARTESIAN_POINT ( 'NONE',  ( -1.185589860596527823, 0.3351407497371320376, -0.05695314934232800774 ) ) ;
#13793 = ORIENTED_EDGE ( 'NONE', *, *, #1397, .F. ) ;
#13794 = DIRECTION ( 'NONE',  ( 0.000000000000000000, 1.000000000000000000, 0.000000000000000000 ) ) ;
#13795 = CARTESIAN_POINT ( 'NONE',  ( -0.5576140732134202693, -0.4921259842519685179, 0.2082870074805209248 ) ) ;
#13796 = CARTESIAN_POINT ( 'NONE',  ( -1.181342415325333350, 0.3435647566446739520, 0.05905511811023622659 ) ) ;
#13797 = EDGE_CURVE ( 'NONE', #14935, #8061, #1507, .T. ) ;
#13798 = DIRECTION ( 'NONE',  ( -0.4999999999999919509, 0.000000000000000000, 0.8660254037844432595 ) ) ;
#13799 = ORIENTED_EDGE ( 'NONE', *, *, #4642, .T. ) ;
#13800 = CARTESIAN_POINT ( 'NONE',  ( -0.4516353949179805483, -0.2952755905511811330, 0.1425541239265588345 ) ) ;
#13801 = ORIENTED_EDGE ( 'NONE', *, *, #3753, .T. ) ;
#13802 = EDGE_CURVE ( 'NONE', #12552, #10256, #3779, .T. ) ;
#13803 = ORIENTED_EDGE ( 'NONE', *, *, #1268, .T. ) ;
#13804 = ORIENTED_EDGE ( 'NONE', *, *, #5770, .T. ) ;
#13805 = CARTESIAN_POINT ( 'NONE',  ( 0.000000000000000000, 0.007874015748031480341, 0.1653543307086614012 ) ) ;
#13806 = FACE_OUTER_BOUND ( 'NONE', #12860, .T. ) ;
#13807 = CARTESIAN_POINT ( 'NONE',  ( -0.002322522588111458446, 0.1532890258252369575, 0.0007019553870511914279 ) ) ;
#13808 = FACE_OUTER_BOUND ( 'NONE', #3507, .T. ) ;
#13809 = APPLICATION_PROTOCOL_DEFINITION ( 'draft international standard', 'automotive_design', 1998, #11291 ) ;
#13810 = DIRECTION ( 'NONE',  ( 0.000000000000000000, 0.000000000000000000, 1.000000000000000000 ) ) ;
#13811 = DIRECTION ( 'NONE',  ( 4.336808689942006692E-15, 0.000000000000000000, -1.000000000000000000 ) ) ;
#13812 = ORIENTED_EDGE ( 'NONE', *, *, #14286, .T. ) ;
#13813 = CARTESIAN_POINT ( 'NONE',  ( -2.111626822439224060, -2.421545435136615687, -0.1175637245596493491 ) ) ;
#13814 = DIRECTION ( 'NONE',  ( -0.8144815189573203495, 0.5801894994542524664, 1.283760644411384150E-16 ) ) ;
#13815 = EDGE_CURVE ( 'NONE', #9431, #11475, #1658, .T. ) ;
#13816 = DIRECTION ( 'NONE',  ( -1.000000000000000000, 0.000000000000000000, -0.000000000000000000 ) ) ;
#13817 = EDGE_LOOP ( 'NONE', ( #7701, #4797, #5661 ) ) ;
#13818 = EDGE_LOOP ( 'NONE', ( #1237, #4560, #14844, #12296, #8229 ) ) ;
#13819 = EDGE_CURVE ( 'NONE', #14414, #9446, #4670, .T. ) ;
#13820 = ORIENTED_EDGE ( 'NONE', *, *, #4444, .F. ) ;
#13821 = ORIENTED_EDGE ( 'NONE', *, *, #10282, .T. ) ;
#13822 = DIRECTION ( 'NONE',  ( 0.4999999999999966693, 0.000000000000000000, 0.8660254037844405950 ) ) ;
#13823 = CARTESIAN_POINT ( 'NONE',  ( -2.029388000666335845, -2.456681529620341475, -0.1220450449751008942 ) ) ;
#13824 = DIRECTION ( 'NONE',  ( -0.000000000000000000, -0.000000000000000000, -1.000000000000000000 ) ) ;
#13825 = CARTESIAN_POINT ( 'NONE',  ( -1.936923698693393536, -2.916673061415975265, -0.1029210798408209532 ) ) ;
#13826 = DIRECTION ( 'NONE',  ( -0.5000000000000004441, -0.000000000000000000, 0.8660254037844382635 ) ) ;
#13827 = DIRECTION ( 'NONE',  ( 0.08188191145424328354, 0.000000000000000000, -0.9966420383350280687 ) ) ;
#13828 = ADVANCED_FACE ( 'NONE', ( #106 ), #11947, .T. ) ;
#13829 = DIRECTION ( 'NONE',  ( 3.476578583725179813E-16, 0.000000000000000000, -1.000000000000000000 ) ) ;
#13830 = CARTESIAN_POINT ( 'NONE',  ( 0.1724006475077543565, -0.1023622047244094474, 0.1728816592724491952 ) ) ;
#13831 = AXIS2_PLACEMENT_3D ( 'NONE', #14716, #1395, #5133 ) ;
#13832 = ORIENTED_EDGE ( 'NONE', *, *, #14480, .T. ) ;
#13833 = AXIS2_PLACEMENT_3D ( 'NONE', #1478, #14719, #3980 ) ;
#13834 = EDGE_CURVE ( 'NONE', #2262, #13144, #6256, .T. ) ;
#13835 = ORIENTED_EDGE ( 'NONE', *, *, #12483, .T. ) ;
#13836 = AXIS2_PLACEMENT_3D ( 'NONE', #2703, #4024, #14609 ) ;
#13837 = ORIENTED_EDGE ( 'NONE', *, *, #3960, .T. ) ;
#13838 = ORIENTED_EDGE ( 'NONE', *, *, #1397, .T. ) ;
#13839 = B_SPLINE_CURVE_WITH_KNOTS ( 'NONE', 3,
 ( #12389, #1661, #13255, #100, #1341 ),
 .UNSPECIFIED., .F., .F.,
 ( 4, 1, 4 ),
 ( 2.432568093613678012E-07, 0.001154943795188613379, 0.002309644333567865190 ),
 .UNSPECIFIED. ) ;
#13840 = ADVANCED_FACE ( 'NONE', ( #7294 ), #7455, .T. ) ;
#13841 = FACE_OUTER_BOUND ( 'NONE', #6502, .T. ) ;
#13842 = DIRECTION ( 'NONE',  ( 0.000000000000000000, 0.000000000000000000, -1.000000000000000000 ) ) ;
#13843 = AXIS2_PLACEMENT_3D ( 'NONE', #833, #4516, #14244 ) ;
#13844 = AXIS2_PLACEMENT_3D ( 'NONE', #12744, #6765, #11553 ) ;
#13845 = FACE_OUTER_BOUND ( 'NONE', #3018, .T. ) ;
#13846 = CIRCLE ( 'NONE', #8087, 0.007874015748031499423 ) ;
#13847 = CARTESIAN_POINT ( 'NONE',  ( 0.000000000000000000, 1.645669291338583085, -0.7007874015748031260 ) ) ;
#13848 = DIRECTION ( 'NONE',  ( 0.000000000000000000, 0.000000000000000000, -1.000000000000000000 ) ) ;
#13849 = AXIS2_PLACEMENT_3D ( 'NONE', #575, #9042, #5336 ) ;
#13850 = CARTESIAN_POINT ( 'NONE',  ( -0.2362204724409448231, -0.02638708502139245488, 0.03937007874015747977 ) ) ;
#13851 = CARTESIAN_POINT ( 'NONE',  ( -1.960453476960047681, -2.761858712000560434, -0.1772931260763774275 ) ) ;
#13852 = ORIENTED_EDGE ( 'NONE', *, *, #7891, .T. ) ;
#13853 = CARTESIAN_POINT ( 'NONE',  ( -0.1629063847838169987, -0.1023622047244094474, 0.2122517380126066888 ) ) ;
#13854 = DIRECTION ( 'NONE',  ( -0.000000000000000000, -1.000000000000000000, -0.000000000000000000 ) ) ;
#13855 = VERTEX_POINT ( 'NONE', #3847 ) ;
#13856 = VERTEX_POINT ( 'NONE', #9894 ) ;
#13857 = TOROIDAL_SURFACE ( 'NONE', #355, 0.5590551181102362266, 0.007874015748031495954 ) ;
#13858 = CIRCLE ( 'NONE', #8100, 0.03543307086614173179 ) ;
#13859 = CIRCLE ( 'NONE', #8864, 0.003937007874015746242 ) ;
#13860 = TOROIDAL_SURFACE ( 'NONE', #14617, 0.1240157480314959815, 0.003937007874015747977 ) ;
#13861 = ORIENTED_EDGE ( 'NONE', *, *, #9352, .F. ) ;
#13862 = VECTOR ( 'NONE', #4865, 39.37007874015748143 ) ;
#13863 = CARTESIAN_POINT ( 'NONE',  ( -1.293236445124221312, 0.1355266887446167634, 0.05905511811023622659 ) ) ;
#13864 = ADVANCED_FACE ( 'NONE', ( #12021 ), #14994, .T. ) ;
#13865 = DIRECTION ( 'NONE',  ( 0.4999999999999995004, 0.000000000000000000, 0.8660254037844390407 ) ) ;
#13866 = CARTESIAN_POINT ( 'NONE',  ( -1.431036756819011213, -0.02829858486107876200, 0.08366141732283460808 ) ) ;
#13867 = FACE_OUTER_BOUND ( 'NONE', #811, .T. ) ;
#13868 = CIRCLE ( 'NONE', #10620, 0.003937007874015750579 ) ;
#13869 = DIRECTION ( 'NONE',  ( -1.000000000000000000, 0.000000000000000000, 0.000000000000000000 ) ) ;
#13870 = VECTOR ( 'NONE', #10619, 39.37007874015748143 ) ;
#13871 = ORIENTED_EDGE ( 'NONE', *, *, #1236, .T. ) ;
#13872 = DIRECTION ( 'NONE',  ( 0.8660254037844383745, 0.000000000000000000, -0.5000000000000004441 ) ) ;
#13873 = AXIS2_PLACEMENT_3D ( 'NONE', #783, #6796, #15277 ) ;
#13874 = DIRECTION ( 'NONE',  ( 0.000000000000000000, 0.000000000000000000, 1.000000000000000000 ) ) ;
#13875 = AXIS2_PLACEMENT_3D ( 'NONE', #7272, #1551, #7506 ) ;
#13876 = CARTESIAN_POINT ( 'NONE',  ( -1.417802900492933782, -0.04287136159519135820, -0.07874015748031495954 ) ) ;
#13877 = DIRECTION ( 'NONE',  ( -1.000000000000000000, 0.000000000000000000, 0.000000000000000000 ) ) ;
#13878 = ORIENTED_EDGE ( 'NONE', *, *, #1408, .F. ) ;
#13879 = DIRECTION ( 'NONE',  ( 0.000000000000000000, 0.000000000000000000, -1.000000000000000000 ) ) ;
#13880 = ORIENTED_EDGE ( 'NONE', *, *, #13532, .T. ) ;
#13882 = EDGE_LOOP ( 'NONE', ( #9279, #3382, #1953, #12242, #13460, #12605, #4129, #6143 ) ) ;
#13881 = CIRCLE ( 'NONE', #6101, 0.04330708661417331101 ) ;
#13883 = CIRCLE ( 'NONE', #3875, 0.007874015748031516770 ) ;
#13884 = CIRCLE ( 'NONE', #7126, 0.05905511811023627516 ) ;
#13885 = CARTESIAN_POINT ( 'NONE',  ( -1.985311755390524624, -2.772329397582317778, 0.1771653543307079026 ) ) ;
#13886 = CARTESIAN_POINT ( 'NONE',  ( -0.1181102362204724254, 2.448818897637795367, -0.03937007874015747977 ) ) ;
#13887 = FACE_OUTER_BOUND ( 'NONE', #10696, .T. ) ;
#13888 = CARTESIAN_POINT ( 'NONE',  ( -0.4769054117961255002, -0.1023622047244094474, 0.3480785096661502265 ) ) ;
#13889 = CYLINDRICAL_SURFACE ( 'NONE', #1201, 0.5511811023622046335 ) ;
#13890 = LINE ( 'NONE', #4411, #5115 ) ;
#13891 = VERTEX_POINT ( 'NONE', #1280 ) ;
#13892 = DIRECTION ( 'NONE',  ( -0.8660254037844383745, 0.000000000000000000, -0.5000000000000002220 ) ) ;
#13893 = EDGE_CURVE ( 'NONE', #1166, #14956, #4168, .T. ) ;
#13894 = DIRECTION ( 'NONE',  ( 0.000000000000000000, 0.000000000000000000, 1.000000000000000000 ) ) ;
#13895 = AXIS2_PLACEMENT_3D ( 'NONE', #10198, #6652, #10267 ) ;
#13896 = CIRCLE ( 'NONE', #7139, 0.7007874015748031260 ) ;
#13897 = AXIS2_PLACEMENT_3D ( 'NONE', #4926, #13069, #11916 ) ;
#13898 = DIRECTION ( 'NONE',  ( 0.000000000000000000, 0.000000000000000000, -1.000000000000000000 ) ) ;
#13899 = VERTEX_POINT ( 'NONE', #7231 ) ;
#13900 = AXIS2_PLACEMENT_3D ( 'NONE', #4282, #6482, #8933 ) ;
#13901 = ORIENTED_EDGE ( 'NONE', *, *, #59, .F. ) ;
#13902 = DIRECTION ( 'NONE',  ( 0.000000000000000000, 0.000000000000000000, -1.000000000000000000 ) ) ;
#13903 = VERTEX_POINT ( 'NONE', #8406 ) ;
#13904 = ORIENTED_EDGE ( 'NONE', *, *, #8976, .F. ) ;
#13905 = ADVANCED_FACE ( 'NONE', ( #2590, #2455 ), #12170, .F. ) ;
#13906 = AXIS2_PLACEMENT_3D ( 'NONE', #1677, #8880, #8725 ) ;
#13907 = AXIS2_PLACEMENT_3D ( 'NONE', #6532, #691, #9222 ) ;
#13908 = ADVANCED_FACE ( 'NONE', ( #8632, #13413 ), #2682, .F. ) ;
#13909 = AXIS2_PLACEMENT_3D ( 'NONE', #1362, #14528, #3789 ) ;
#13910 = DIRECTION ( 'NONE',  ( 0.000000000000000000, 1.000000000000000000, 0.000000000000000000 ) ) ;
#13911 = CARTESIAN_POINT ( 'NONE',  ( -0.06692913385815735250, -0.4921259842519685179, -0.5870514566507987197 ) ) ;
#13912 =( NAMED_UNIT ( * ) SI_UNIT ( $, .STERADIAN. ) SOLID_ANGLE_UNIT ( ) );
#13913 = TOROIDAL_SURFACE ( 'NONE', #14166, 0.1240157480314959815, 0.003937007874015747977 ) ;
#13914 = PRODUCT_DEFINITION_SHAPE ( 'NONE', 'NONE',  #15321 ) ;
#13915 = LINE ( 'NONE', #10467, #6950 ) ;
#13916 = EDGE_CURVE ( 'NONE', #12552, #15201, #11680, .T. ) ;
#13917 = DIRECTION ( 'NONE',  ( 0.000000000000000000, 0.000000000000000000, -1.000000000000000000 ) ) ;
#13918 = DIRECTION ( 'NONE',  ( -1.000000000000000000, -0.000000000000000000, -0.000000000000000000 ) ) ;
#13919 = CARTESIAN_POINT ( 'NONE',  ( 0.000000000000000000, 0.3149606299212598381, 0.000000000000000000 ) ) ;
#13920 = DIRECTION ( 'NONE',  ( -1.000000000000000000, 0.000000000000000000, 0.000000000000000000 ) ) ;
#13921 = AXIS2_PLACEMENT_3D ( 'NONE', #2941, #15008, #1994 ) ;
#13922 = ORIENTED_EDGE ( 'NONE', *, *, #3154, .F. ) ;
#13923 = ORIENTED_EDGE ( 'NONE', *, *, #9361, .F. ) ;
#13924 = EDGE_LOOP ( 'NONE', ( #14726, #3709, #56, #5414 ) ) ;
#13925 = VECTOR ( 'NONE', #4254, 39.37007874015748143 ) ;
#13926 = VERTEX_POINT ( 'NONE', #13647 ) ;
#13927 = EDGE_CURVE ( 'NONE', #11529, #556, #8680, .T. ) ;
#13928 = EDGE_CURVE ( 'NONE', #10377, #7046, #4415, .T. ) ;
#13929 = CARTESIAN_POINT ( 'NONE',  ( 8.100026073100603114E-17, 1.606299212598425674, -0.6614173228346456046 ) ) ;
#13930 = DIRECTION ( 'NONE',  ( 0.000000000000000000, 1.000000000000000000, 0.000000000000000000 ) ) ;
#13931 = AXIS2_PLACEMENT_3D ( 'NONE', #12176, #6035, #5094 ) ;
#13932 = DIRECTION ( 'NONE',  ( -0.000000000000000000, -1.000000000000000000, -0.000000000000000000 ) ) ;
#13933 = ADVANCED_FACE ( 'NONE', ( #8784 ), #4684, .T. ) ;
#13934 = CARTESIAN_POINT ( 'NONE',  ( -0.07002222008683997578, -0.1674826920712330913, -0.05905511811023624741 ) ) ;
#13935 = LINE ( 'NONE', #13709, #3185 ) ;
#13936 = CIRCLE ( 'NONE', #8184, 0.03937007874015751446 ) ;
#13937 = CARTESIAN_POINT ( 'NONE',  ( -1.946192867917151847, -2.743611295743893397, -0.1749236412511677441 ) ) ;
#13938 = ORIENTED_EDGE ( 'NONE', *, *, #8641, .F. ) ;
#13939 = CARTESIAN_POINT ( 'NONE',  ( 0.06351958502452506594, -0.1023622047244094474, -0.2357441700067326729 ) ) ;
#13940 = DIRECTION ( 'NONE',  ( 0.000000000000000000, 0.000000000000000000, 1.000000000000000000 ) ) ;
#13941 = DIRECTION ( 'NONE',  ( 1.000000000000000000, 0.000000000000000000, 1.445602896647339903E-16 ) ) ;
#13942 = ORIENTED_EDGE ( 'NONE', *, *, #13174, .F. ) ;
#13943 = ORIENTED_EDGE ( 'NONE', *, *, #9254, .T. ) ;
#13944 = AXIS2_PLACEMENT_3D ( 'NONE', #6784, #14966, #8934 ) ;
#13945 = CIRCLE ( 'NONE', #7187, 0.03937007874015751446 ) ;
#13946 = EDGE_LOOP ( 'NONE', ( #10077, #7480 ) ) ;
#13947 = LINE ( 'NONE', #6645, #5354 ) ;
#13948 = CIRCLE ( 'NONE', #6934, 0.003937007874015737569 ) ;
#13949 = CARTESIAN_POINT ( 'NONE',  ( -0.06351958502436047538, -0.1023622047244094474, -0.2357441700068276802 ) ) ;
#13950 = CARTESIAN_POINT ( 'NONE',  ( 0.000000000000000000, 0.000000000000000000, -0.5511811023622046335 ) ) ;
#13951 = EDGE_CURVE ( 'NONE', #13266, #12883, #14435, .T. ) ;
#13953 = TOROIDAL_SURFACE ( 'NONE', #7199, 0.1653543307086614012, 0.007874015748031495954 ) ;
#13952 = DIRECTION ( 'NONE',  ( -5.204170427930408030E-14, 0.000000000000000000, -1.000000000000000000 ) ) ;
#13954 = DIRECTION ( 'NONE',  ( -1.000000000000000000, -0.000000000000000000, -1.445602896647339903E-16 ) ) ;
#13955 = ORIENTED_EDGE ( 'NONE', *, *, #11796, .F. ) ;
#13956 = DIRECTION ( 'NONE',  ( 0.000000000000000000, 0.000000000000000000, -1.000000000000000000 ) ) ;
#13957 = DIRECTION ( 'NONE',  ( -0.000000000000000000, -0.000000000000000000, -1.000000000000000000 ) ) ;
#13958 = CIRCLE ( 'NONE', #8959, 0.003937007874015724558 ) ;
#13959 = DIRECTION ( 'NONE',  ( -1.000000000000000000, 0.000000000000000000, 0.000000000000000000 ) ) ;
#13960 = EDGE_CURVE ( 'NONE', #877, #15414, #9182, .T. ) ;
#13961 = LINE ( 'NONE', #874, #1097 ) ;
#13962 = VERTEX_POINT ( 'NONE', #14755 ) ;
#13963 = ADVANCED_FACE ( 'NONE', ( #11215 ), #1740, .F. ) ;
#13964 = DIRECTION ( 'NONE',  ( 1.000000000000000000, 0.000000000000000000, 0.000000000000000000 ) ) ;
#13965 = ORIENTED_EDGE ( 'NONE', *, *, #1053, .T. ) ;
#13966 = ORIENTED_EDGE ( 'NONE', *, *, #8763, .F. ) ;
#13967 = VECTOR ( 'NONE', #12167, 39.37007874015748143 ) ;
#13968 = VERTEX_POINT ( 'NONE', #8863 ) ;
#13969 = CARTESIAN_POINT ( 'NONE',  ( 0.000000000000000000, -1.707404996040164512E-17, 0.1653543307086614012 ) ) ;
#13970 = DIRECTION ( 'NONE',  ( -1.000000000000000000, 0.000000000000000000, 0.000000000000000000 ) ) ;
#13971 = AXIS2_PLACEMENT_3D ( 'NONE', #4818, #6150, #13515 ) ;
#13972 = CARTESIAN_POINT ( 'NONE',  ( -0.05072818602969170199, 0.1683578795566404995, -0.03094016780478001452 ) ) ;
#13973 = DIRECTION ( 'NONE',  ( -1.000000000000000000, 0.000000000000000000, 0.000000000000000000 ) ) ;
#13974 = ITEM_DEFINED_TRANSFORMATION ( 'NONE', 'NONE', #373,  #11481 ) ;
#13975 = FACE_OUTER_BOUND ( 'NONE', #14457, .T. ) ;
#13976 = CARTESIAN_POINT ( 'NONE',  ( -0.04711866733795021939, -0.1840656518295271660, 0.03212400068286348082 ) ) ;
#13977 = ORIENTED_EDGE ( 'NONE', *, *, #10836, .T. ) ;
#13978 = DIRECTION ( 'NONE',  ( -0.5000000000000001110, 0.000000000000000000, 0.8660254037844385966 ) ) ;
#13979 = LINE ( 'NONE', #14051, #10847 ) ;
#13980 = DIRECTION ( 'NONE',  ( -0.000000000000000000, 0.000000000000000000, 1.000000000000000000 ) ) ;
#13981 = AXIS2_PLACEMENT_3D ( 'NONE', #4056, #14801, #14563 ) ;
#13982 = DIRECTION ( 'NONE',  ( 0.000000000000000000, 2.212657494868377674E-16, -1.000000000000000000 ) ) ;
#13983 = FILL_AREA_STYLE_COLOUR ( '', #14444 ) ;
#13984 = VERTEX_POINT ( 'NONE', #5404 ) ;
#13985 = VECTOR ( 'NONE', #9702, 39.37007874015748143 ) ;
#13986 = VERTEX_POINT ( 'NONE', #5310 ) ;
#13987 = DIRECTION ( 'NONE',  ( 0.000000000000000000, 2.212657494868377674E-16, 1.000000000000000000 ) ) ;
#13988 = ORIENTED_EDGE ( 'NONE', *, *, #8047, .F. ) ;
#13989 = ORIENTED_EDGE ( 'NONE', *, *, #14448, .T. ) ;
#13990 = DIRECTION ( 'NONE',  ( 0.000000000000000000, -0.000000000000000000, 1.000000000000000000 ) ) ;
#13991 = CARTESIAN_POINT ( 'NONE',  ( -1.990392212731196375, -2.816401147560732898, 0.1718120134069966720 ) ) ;
#13992 = CARTESIAN_POINT ( 'NONE',  ( 0.5610236220472175628, -0.4881889763779528324, 0.2102555114175294892 ) ) ;
#13993 = LINE ( 'NONE', #1156, #9663 ) ;
#13994 = CARTESIAN_POINT ( 'NONE',  ( -1.401197114347125794, -0.004216232782927999655, 0.05905511811023622659 ) ) ;
#13995 = EDGE_CURVE ( 'NONE', #6393, #11911, #10038, .T. ) ;
#13996 = DIRECTION ( 'NONE',  ( 0.8011800915434493797, -0.5984233124757342148, 0.000000000000000000 ) ) ;
#13997 = CYLINDRICAL_SURFACE ( 'NONE', #5652, 0.007874015748031482076 ) ;
#13998 = EDGE_CURVE ( 'NONE', #2247, #692, #727, .T. ) ;
#13999 = ORIENTED_EDGE ( 'NONE', *, *, #5648, .F. ) ;
#14000 = ORIENTED_EDGE ( 'NONE', *, *, #10687, .T. ) ;
#14001 = VERTEX_POINT ( 'NONE', #496 ) ;
#14002 = ORIENTED_EDGE ( 'NONE', *, *, #5267, .T. ) ;
#14003 = ADVANCED_FACE ( 'NONE', ( #4074 ), #10117, .T. ) ;
#14004 = APPLICATION_CONTEXT ( 'automotive_design' ) ;
#14005 = DIRECTION ( 'NONE',  ( -4.336808689942014285E-16, 0.000000000000000000, 1.000000000000000000 ) ) ;
#14006 = DIRECTION ( 'NONE',  ( -1.000000000000000000, -0.000000000000000000, -0.000000000000000000 ) ) ;
#14007 = CARTESIAN_POINT ( 'NONE',  ( -0.07500546397816790223, 0.1646499958011359843, 0.03937007824588655003 ) ) ;
#14008 = CARTESIAN_POINT ( 'NONE',  ( 0.4751993499420012479, 1.346456692913385877, 0.3506226965216235336 ) ) ;
#14009 = DIRECTION ( 'NONE',  ( 0.000000000000000000, 1.000000000000000000, 0.000000000000000000 ) ) ;
#14010 = CARTESIAN_POINT ( 'NONE',  ( -0.06299212598414161146, -0.2952755905511811330, -0.3757906139821208247 ) ) ;
#14011 = CARTESIAN_POINT ( 'NONE',  ( -1.930618484338028740, -2.788977046644874669, -0.1558575928594421456 ) ) ;
#14012 = ORIENTED_EDGE ( 'NONE', *, *, #9597, .F. ) ;
#14013 = CARTESIAN_POINT ( 'NONE',  ( -0.2952755905511810219, -0.02638708502139244794, -0.03937007874015747977 ) ) ;
#14014 = ADVANCED_FACE ( 'NONE', ( #5239 ), #2913, .F. ) ;
#14015 = CARTESIAN_POINT ( 'NONE',  ( -0.5610236220472173407, -0.4881889763779528324, 0.2102555114175287954 ) ) ;
#14016 = EDGE_CURVE ( 'NONE', #7217, #7115, #13681, .T. ) ;
#14017 = ORIENTED_EDGE ( 'NONE', *, *, #6388, .F. ) ;
#14018 = ORIENTED_EDGE ( 'NONE', *, *, #171, .T. ) ;
#14019 = EDGE_CURVE ( 'NONE', #624, #14199, #5411, .T. ) ;
#14020 = EDGE_LOOP ( 'NONE', ( #7212, #2602, #9770, #7063 ) ) ;
#14021 = FACE_OUTER_BOUND ( 'NONE', #5577, .T. ) ;
#14022 = DIRECTION ( 'NONE',  ( -0.000000000000000000, 0.000000000000000000, 1.000000000000000000 ) ) ;
#14023 = CARTESIAN_POINT ( 'NONE',  ( -1.978181763874820032, -2.794902419994705234, 0.1760903034428087099 ) ) ;
#14024 = DIRECTION ( 'NONE',  ( 0.000000000000000000, 0.000000000000000000, -1.000000000000000000 ) ) ;
#14025 = CARTESIAN_POINT ( 'NONE',  ( 0.000000000000000000, 0.000000000000000000, 0.000000000000000000 ) ) ;
#14026 = DIRECTION ( 'NONE',  ( 1.000000000000000000, 1.734723475976817507E-14, 0.000000000000000000 ) ) ;
#14027 = EDGE_LOOP ( 'NONE', ( #1219, #1057 ) ) ;
#14028 = CARTESIAN_POINT ( 'NONE',  ( 0.5405850968741658935, 1.037100910086334205, 0.2377418676364856376 ) ) ;
#14029 = DIRECTION ( 'NONE',  ( -0.000000000000000000, -1.000000000000000000, -0.000000000000000000 ) ) ;
#14030 = CARTESIAN_POINT ( 'NONE',  ( -0.4765556591342228199, 1.037732670558789483, 0.3487844890899370887 ) ) ;
#14031 = EDGE_CURVE ( 'NONE', #5195, #7046, #1806, .T. ) ;
#14032 = DIRECTION ( 'NONE',  ( 0.4999999999999992228, 0.000000000000000000, 0.8660254037844391517 ) ) ;
#14033 = ORIENTED_EDGE ( 'NONE', *, *, #11307, .T. ) ;
#14034 = CARTESIAN_POINT ( 'NONE',  ( -0.4307978335858689278, -0.003937007874015747977, 0.4279391777402706265 ) ) ;
#14035 = VERTEX_POINT ( 'NONE', #2753 ) ;
#14036 = EDGE_CURVE ( 'NONE', #15416, #5248, #1187, .T. ) ;
#14037 = ADVANCED_FACE ( 'NONE', ( #2205 ), #15281, .T. ) ;
#14038 = ORIENTED_EDGE ( 'NONE', *, *, #5519, .T. ) ;
#14039 = PRODUCT_DEFINITION_SHAPE ( 'NONE', 'NONE',  #15470 ) ;
#14040 = ORIENTED_EDGE ( 'NONE', *, *, #2551, .F. ) ;
#14041 = CARTESIAN_POINT ( 'NONE',  ( 0.000000000000000000, 0.007874015748031480341, 0.000000000000000000 ) ) ;
#14042 = DIRECTION ( 'NONE',  ( -1.000000000000000000, 0.000000000000000000, 0.000000000000000000 ) ) ;
#14043 = EDGE_CURVE ( 'NONE', #15234, #5486, #12776, .T. ) ;
#14044 = DIRECTION ( 'NONE',  ( -0.000000000000000000, -1.000000000000000000, -0.000000000000000000 ) ) ;
#14045 = LINE ( 'NONE', #10592, #362 ) ;
#14046 = CONTEXT_DEPENDENT_SHAPE_REPRESENTATION ( #3000, #7035 ) ;
#14047 = DIRECTION ( 'NONE',  ( -0.000000000000000000, -1.000000000000000000, -0.000000000000000000 ) ) ;
#14048 = CARTESIAN_POINT ( 'NONE',  ( -0.5398975377803494347, -0.4921259842519685179, 0.2389729469846940679 ) ) ;
#14049 = VERTEX_POINT ( 'NONE', #6734 ) ;
#14050 = CYLINDRICAL_SURFACE ( 'NONE', #9930, 0.007874015748031499423 ) ;
#14051 = CARTESIAN_POINT ( 'NONE',  ( -0.2373612774289040883, -0.4921259842519685179, 0.06430355563116459117 ) ) ;
#14052 = DIRECTION ( 'NONE',  ( 1.000000000000000000, 0.000000000000000000, 3.476578583725179813E-16 ) ) ;
#14053 = PRESENTATION_STYLE_ASSIGNMENT (( #2371 ) ) ;
#14054 = DIRECTION ( 'NONE',  ( 0.5000000000000004441, 0.000000000000000000, -0.8660254037844383745 ) ) ;
#14055 = ORIENTED_EDGE ( 'NONE', *, *, #14094, .T. ) ;
#14056 = ORIENTED_EDGE ( 'NONE', *, *, #5670, .F. ) ;
#14057 = DIRECTION ( 'NONE',  ( -1.000000000000000000, -0.000000000000000000, -0.000000000000000000 ) ) ;
#14058 = EDGE_LOOP ( 'NONE', ( #8554, #2982 ) ) ;
#14059 = ORIENTED_EDGE ( 'NONE', *, *, #10139, .F. ) ;
#14060 = ORIENTED_EDGE ( 'NONE', *, *, #39, .F. ) ;
#14061 = DIRECTION ( 'NONE',  ( -0.000000000000000000, -0.000000000000000000, -1.000000000000000000 ) ) ;
#14062 = EDGE_CURVE ( 'NONE', #4029, #10145, #6661, .T. ) ;
#14063 = FACE_OUTER_BOUND ( 'NONE', #11655, .T. ) ;
#14064 = DIRECTION ( 'NONE',  ( -0.5000000000000039968, 0.000000000000000000, -0.8660254037844362651 ) ) ;
#14065 =( CONVERSION_BASED_UNIT ( 'INCH', #6843 ) LENGTH_UNIT ( ) NAMED_UNIT ( #10673 ) );
#14066 = DIRECTION ( 'NONE',  ( 0.000000000000000000, -0.000000000000000000, 1.000000000000000000 ) ) ;
#14067 = ORIENTED_EDGE ( 'NONE', *, *, #7517, .T. ) ;
#14068 = EDGE_LOOP ( 'NONE', ( #4004, #13332, #14361, #12724 ) ) ;
#14069 = ORIENTED_EDGE ( 'NONE', *, *, #5752, .T. ) ;
#14070 = ORIENTED_EDGE ( 'NONE', *, *, #10230, .F. ) ;
#14071 = CARTESIAN_POINT ( 'NONE',  ( 0.7052242655755273093, -1.858423098537180129, -0.08366141732283413623 ) ) ;
#14072 = CARTESIAN_POINT ( 'NONE',  ( -1.511943070284283097, 0.2262540267724840182, 0.03937007874015747977 ) ) ;
#14073 = FACE_OUTER_BOUND ( 'NONE', #15026, .T. ) ;
#14074 = CARTESIAN_POINT ( 'NONE',  ( -0.06427269473108324083, 0.1662356183067242588, 0.05825535267941785861 ) ) ;
#14075 = DIRECTION ( 'NONE',  ( -0.000000000000000000, -0.000000000000000000, -1.000000000000000000 ) ) ;
#14076 = CARTESIAN_POINT ( 'NONE',  ( 2.419703784132994590E-19, 0.07093549527207483607, -0.07900545476875228679 ) ) ;
#14077 = LINE ( 'NONE', #8134, #10580 ) ;
#14078 = AXIS2_PLACEMENT_3D ( 'NONE', #4980, #7261, #7413 ) ;
#14079 = EDGE_LOOP ( 'NONE', ( #12722, #2771, #15347, #11182 ) ) ;
#14080 = CARTESIAN_POINT ( 'NONE',  ( -1.496171808639726875, 0.2144740403064263057, 0.03937007874015747977 ) ) ;
#14081 = AXIS2_PLACEMENT_3D ( 'NONE', #8752, #12055, #11991 ) ;
#14082 = EDGE_CURVE ( 'NONE', #3335, #5966, #7919, .T. ) ;
#14083 = LINE ( 'NONE', #5929, #5835 ) ;
#14084 = CARTESIAN_POINT ( 'NONE',  ( -0.5576140732134202693, -0.4921259842519685179, 0.2082870074805209526 ) ) ;
#14085 = ORIENTED_EDGE ( 'NONE', *, *, #5754, .F. ) ;
#14086 = VERTEX_POINT ( 'NONE', #6978 ) ;
#14087 = ORIENTED_EDGE ( 'NONE', *, *, #7042, .F. ) ;
#14088 = CIRCLE ( 'NONE', #2576, 0.04330708661417331101 ) ;
#14089 = AXIS2_PLACEMENT_3D ( 'NONE', #13911, #12809, #3181 ) ;
#14090 = CARTESIAN_POINT ( 'NONE',  ( 0.4591888763630541104, -0.4921259842519685179, 0.3787644491703230365 ) ) ;
#14091 = VECTOR ( 'NONE', #5547, 39.37007874015748143 ) ;
#14092 = EDGE_CURVE ( 'NONE', #1546, #1436, #1671, .T. ) ;
#14093 = CIRCLE ( 'NONE', #12338, 0.007874015748031516770 ) ;
#14094 = EDGE_CURVE ( 'NONE', #5898, #12947, #6402, .T. ) ;
#14095 = CARTESIAN_POINT ( 'NONE',  ( -0.5899421238646493926, -0.003937007874015747977, 0.1591122789105256785 ) ) ;
#14096 = CYLINDRICAL_SURFACE ( 'NONE', #8371, 3.169291338582677753 ) ;
#14097 = DIRECTION ( 'NONE',  ( 1.000000000000000000, 0.000000000000000000, 0.000000000000000000 ) ) ;
#14098 = CARTESIAN_POINT ( 'NONE',  ( -1.190198933766848377, 0.3259758027579584549, -0.05905511811023622659 ) ) ;
#14099 = VERTEX_POINT ( 'NONE', #5545 ) ;
#14100 = DIRECTION ( 'NONE',  ( 0.4999999999999979461, 0.000000000000000000, 0.8660254037844398178 ) ) ;
#14101 = EDGE_CURVE ( 'NONE', #7333, #3058, #7083, .T. ) ;
#14102 = DIRECTION ( 'NONE',  ( 1.000000000000000000, 0.000000000000000000, 0.000000000000000000 ) ) ;
#14103 = AXIS2_PLACEMENT_3D ( 'NONE', #2714, #5126, #8808 ) ;
#14104 = AXIS2_PLACEMENT_3D ( 'NONE', #11639, #10464, #6688 ) ;
#14105 = DIRECTION ( 'NONE',  ( 0.000000000000000000, 0.000000000000000000, 1.000000000000000000 ) ) ;
#14106 = CARTESIAN_POINT ( 'NONE',  ( -1.602365476182131099, 0.1047621256497578840, 0.05341113178340452933 ) ) ;
#14107 = ORIENTED_EDGE ( 'NONE', *, *, #12734, .T. ) ;
#14108 = CIRCLE ( 'NONE', #600, 0.1240157480314959260 ) ;
#14109 = DIRECTION ( 'NONE',  ( 0.4274092037376938102, 0.000000000000000000, 0.9040582794047684612 ) ) ;
#14110 = VECTOR ( 'NONE', #10431, 39.37007874015748143 ) ;
#14111 = ORIENTED_EDGE ( 'NONE', *, *, #6760, .T. ) ;
#14112 = EDGE_LOOP ( 'NONE', ( #13528, #14069, #3942, #10672 ) ) ;
#14113 = EDGE_CURVE ( 'NONE', #7462, #13020, #10573, .T. ) ;
#14114 = FACE_OUTER_BOUND ( 'NONE', #8492, .T. ) ;
#14115 = DIRECTION ( 'NONE',  ( -0.8660254037844405950, -4.336808689942015369E-15, -0.4999999999999967804 ) ) ;
#14116 = TOROIDAL_SURFACE ( 'NONE', #2103, 0.6614173228346456046, 0.007874015748031495954 ) ;
#14117 = CIRCLE ( 'NONE', #4607, 0.01968503937007871907 ) ;
#14118 = EDGE_CURVE ( 'NONE', #4762, #9720, #10690, .T. ) ;
#14119 = TOROIDAL_SURFACE ( 'NONE', #4322, 0.04330708661417326938, 0.003937007874015747977 ) ;
#14120 = VECTOR ( 'NONE', #1189, 39.37007874015748143 ) ;
#14121 = CARTESIAN_POINT ( 'NONE',  ( -0.04489243112415652881, 0.1480120765563566754, -0.05194558739575130119 ) ) ;
#14122 = DIRECTION ( 'NONE',  ( 1.445602896647339903E-16, 0.000000000000000000, -1.000000000000000000 ) ) ;
#14123 = CIRCLE ( 'NONE', #14367, 0.01968503937007875723 ) ;
#14124 = LINE ( 'NONE', #7061, #455 ) ;
#14125 = AXIS2_PLACEMENT_3D ( 'NONE', #6582, #11383, #4249 ) ;
#14126 = FACE_OUTER_BOUND ( 'NONE', #4941, .T. ) ;
#14128 = VERTEX_POINT ( 'NONE', #9417 ) ;
#14127 = AXIS2_PLACEMENT_3D ( 'NONE', #12101, #13272, #1453 ) ;
#14129 = EDGE_CURVE ( 'NONE', #7462, #13509, #5657, .T. ) ;
#14130 = FACE_BOUND ( 'NONE', #6470, .T. ) ;
#14131 = FACE_OUTER_BOUND ( 'NONE', #5521, .T. ) ;
#14132 = LENGTH_MEASURE_WITH_UNIT ( LENGTH_MEASURE( 0.02539999999999999897 ), #13103 );
#14133 = ORIENTED_EDGE ( 'NONE', *, *, #4945, .T. ) ;
#14134 = VECTOR ( 'NONE', #10286, 39.37007874015749564 ) ;
#14135 = AXIS2_PLACEMENT_3D ( 'NONE', #1605, #2848, #1692 ) ;
#14136 = CIRCLE ( 'NONE', #13636, 0.01968503937007876417 ) ;
#14137 = ORIENTED_EDGE ( 'NONE', *, *, #9611, .T. ) ;
#14138 = ADVANCED_FACE ( 'NONE', ( #14190 ), #3460, .F. ) ;
#14139 = CARTESIAN_POINT ( 'NONE',  ( 0.5445274672588121812, 1.043263280880422528, 0.2461921031270739857 ) ) ;
#14140 = ORIENTED_EDGE ( 'NONE', *, *, #1581, .F. ) ;
#14141 = CIRCLE ( 'NONE', #872, 0.5511811023622046335 ) ;
#14142 = EDGE_LOOP ( 'NONE', ( #13087, #605, #583, #1938 ) ) ;
#14143 = VERTEX_POINT ( 'NONE', #2272 ) ;
#14144 = DIRECTION ( 'NONE',  ( 0.000000000000000000, 0.000000000000000000, 1.000000000000000000 ) ) ;
#14145 = DIRECTION ( 'NONE',  ( 0.000000000000000000, 0.000000000000000000, 1.000000000000000000 ) ) ;
#14146 = CYLINDRICAL_SURFACE ( 'NONE', #1095, 0.1279527559055117780 ) ;
#14147 =( LENGTH_UNIT ( ) NAMED_UNIT ( * ) SI_UNIT ( $, .METRE. ) );
#14148 = AXIS2_PLACEMENT_3D ( 'NONE', #15046, #10428, #15121 ) ;
#14149 = VECTOR ( 'NONE', #12479, 39.37007874015748143 ) ;
#14150 = LINE ( 'NONE', #12745, #5178 ) ;
#14151 = DIRECTION ( 'NONE',  ( 1.000000000000000000, -3.469446951953611428E-15, 0.000000000000000000 ) ) ;
#14152 = EDGE_CURVE ( 'NONE', #12616, #2098, #7995, .T. ) ;
#14153 = DIRECTION ( 'NONE',  ( 0.000000000000000000, 0.000000000000000000, -1.000000000000000000 ) ) ;
#14154 = CIRCLE ( 'NONE', #4377, 3.149606299212599048 ) ;
#14155 = DIRECTION ( 'NONE',  ( 0.000000000000000000, 0.000000000000000000, -1.000000000000000000 ) ) ;
#14156 = FACE_OUTER_BOUND ( 'NONE', #530, .T. ) ;
#14157 = ADVANCED_FACE ( 'NONE', ( #15211 ), #7047, .T. ) ;
#14158 = EDGE_LOOP ( 'NONE', ( #4221, #12069, #2490 ) ) ;
#14159 = EDGE_CURVE ( 'NONE', #1302, #2464, #13936, .T. ) ;
#14160 = ORIENTED_EDGE ( 'NONE', *, *, #3196, .T. ) ;
#14161 = AXIS2_PLACEMENT_3D ( 'NONE', #13689, #14854, #1772 ) ;
#14162 = VERTEX_POINT ( 'NONE', #12846 ) ;
#14163 = CIRCLE ( 'NONE', #9673, 0.5984251968503937480 ) ;
#14164 = CIRCLE ( 'NONE', #1401, 0.003937007874015741038 ) ;
#14165 = ORIENTED_EDGE ( 'NONE', *, *, #2616, .F. ) ;
#14166 = AXIS2_PLACEMENT_3D ( 'NONE', #3652, #8426, #12104 ) ;
#14167 = CYLINDRICAL_SURFACE ( 'NONE', #11867, 0.01968503937007871907 ) ;
#14168 = CARTESIAN_POINT ( 'NONE',  ( -0.08151194962748882500, 0.1637246173173400321, 0.03937007874015747977 ) ) ;
#14169 = CARTESIAN_POINT ( 'NONE',  ( -0.02371960882139430987, -0.1628608293428424891, -0.03730919803856837247 ) ) ;
#14170 = DIRECTION ( 'NONE',  ( 0.5000000000000001110, 0.000000000000000000, -0.8660254037844385966 ) ) ;
#14171 = AXIS2_PLACEMENT_3D ( 'NONE', #9466, #10624, #12814 ) ;
#14172 = CARTESIAN_POINT ( 'NONE',  ( 0.4822834645669299980, -0.09448818897637796532, 0.3466374647693609146 ) ) ;
#14173 = ORIENTED_EDGE ( 'NONE', *, *, #3664, .F. ) ;
#14174 = LINE ( 'NONE', #12919, #3443 ) ;
#14175 = LINE ( 'NONE', #9309, #15380 ) ;
#14176 = CARTESIAN_POINT ( 'NONE',  ( -0.03450359373084976866, 0.06995722947081559062, 0.07617071561662558388 ) ) ;
#14177 = AXIS2_PLACEMENT_3D ( 'NONE', #10598, #5727, #15303 ) ;
#14178 = ORIENTED_EDGE ( 'NONE', *, *, #11999, .F. ) ;
#14179 = EDGE_LOOP ( 'NONE', ( #3155, #13538, #5737, #13578 ) ) ;
#14180 = VERTEX_POINT ( 'NONE', #2118 ) ;
#14181 = AXIS2_PLACEMENT_3D ( 'NONE', #13672, #514, #13898 ) ;
#14182 = PLANE ( 'NONE',  #7611 ) ;
#14183 = AXIS2_PLACEMENT_3D ( 'NONE', #4391, #11522, #959 ) ;
#14184 = CARTESIAN_POINT ( 'NONE',  ( -0.7455328141524873997, 1.190944881889763884, 0.3622425942647021779 ) ) ;
#14185 = DIRECTION ( 'NONE',  ( -1.000000000000000000, 0.000000000000000000, 0.000000000000000000 ) ) ;
#14186 = CARTESIAN_POINT ( 'NONE',  ( -0.4586614173228354407, -0.1023622047244094474, 0.3875520507749248833 ) ) ;
#14187 = CYLINDRICAL_SURFACE ( 'NONE', #10476, 0.007874015748031499423 ) ;
#14188 = CARTESIAN_POINT ( 'NONE',  ( -1.916768853550577134, -2.896547607920614720, 0.1269301806022984647 ) ) ;
#14189 = EDGE_LOOP ( 'NONE', ( #4419, #11398, #13268, #12918 ) ) ;
#14190 = FACE_OUTER_BOUND ( 'NONE', #3751, .T. ) ;
#14191 = DIRECTION ( 'NONE',  ( 0.8660254037844385966, 0.000000000000000000, 0.5000000000000001110 ) ) ;
#14192 = DIRECTION ( 'NONE',  ( 0.000000000000000000, 1.000000000000000000, 0.000000000000000000 ) ) ;
#14193 = DIRECTION ( 'NONE',  ( -1.000000000000000000, -1.734723475976817507E-14, 0.000000000000000000 ) ) ;
#14194 = ORIENTED_EDGE ( 'NONE', *, *, #918, .F. ) ;
#14195 = EDGE_CURVE ( 'NONE', #3677, #4499, #11430, .T. ) ;
#14196 = CARTESIAN_POINT ( 'NONE',  ( -1.293236445124221312, 0.1355266887446167634, -0.03937007874015747977 ) ) ;
#14197 = AXIS2_PLACEMENT_3D ( 'NONE', #6787, #5466, #8046 ) ;
#14198 = EDGE_CURVE ( 'NONE', #8323, #9995, #11972, .T. ) ;
#14199 = VERTEX_POINT ( 'NONE', #1420 ) ;
#14200 = CIRCLE ( 'NONE', #15204, 0.003937007874015724558 ) ;
#14201 = ORIENTED_EDGE ( 'NONE', *, *, #1026, .T. ) ;
#14202 = VERTEX_POINT ( 'NONE', #6016 ) ;
#14203 = EDGE_CURVE ( 'NONE', #6519, #2233, #10179, .T. ) ;
#14204 = DIRECTION ( 'NONE',  ( -0.000000000000000000, -1.000000000000000000, -0.000000000000000000 ) ) ;
#14205 = LINE ( 'NONE', #10442, #655 ) ;
#14206 = AXIS2_PLACEMENT_3D ( 'NONE', #9617, #13222, #4977 ) ;
#14207 = CARTESIAN_POINT ( 'NONE',  ( -1.417802899857368182, -0.04287136101802047766, 0.07345918205385276734 ) ) ;
#14208 = CARTESIAN_POINT ( 'NONE',  ( -0.4307978335858689278, -0.09842519685039370636, 0.4279391777402706820 ) ) ;
#14209 = SPHERICAL_SURFACE ( 'NONE', #14709, 0.01968503937007873988 ) ;
#14210 = CIRCLE ( 'NONE', #7443, 0.5511811023622046335 ) ;
#14211 = CARTESIAN_POINT ( 'NONE',  ( -1.491640810881974977, 0.2222636556240916161, 0.03937007874015747977 ) ) ;
#14212 = EDGE_LOOP ( 'NONE', ( #5599, #5992, #7558, #1983 ) ) ;
#14213 = CARTESIAN_POINT ( 'NONE',  ( -1.398125690441303304, -0.003404927804347041096, -0.03937007874015747977 ) ) ;
#14214 = DIRECTION ( 'NONE',  ( -0.5163221703236040572, -0.6912615786549138885, 0.5055381749263252456 ) ) ;
#14215 = LINE ( 'NONE', #8017, #3948 ) ;
#14216 = ADVANCED_FACE ( 'NONE', ( #12005 ), #12067, .F. ) ;
#14217 = DIRECTION ( 'NONE',  ( 0.000000000000000000, 0.000000000000000000, -1.000000000000000000 ) ) ;
#14218 = AXIS2_PLACEMENT_3D ( 'NONE', #14443, #15080, #11643 ) ;
#14219 = EDGE_CURVE ( 'NONE', #4395, #5049, #7181, .T. ) ;
#14220 = ORIENTED_EDGE ( 'NONE', *, *, #12944, .T. ) ;
#14221 =( REPRESENTATION_RELATIONSHIP ('NONE','NONE', #8904, #2403 ) REPRESENTATION_RELATIONSHIP_WITH_TRANSFORMATION ( #5496 )SHAPE_REPRESENTATION_RELATIONSHIP( ) );
#14222 = CARTESIAN_POINT ( 'NONE',  ( 0.5084014747882494856, -0.09842519685039370636, 0.2935257283254013583 ) ) ;
#14223 = ORIENTED_EDGE ( 'NONE', *, *, #3755, .T. ) ;
#14224 = VECTOR ( 'NONE', #11218, 39.37007874015748143 ) ;
#14225 = ORIENTED_EDGE ( 'NONE', *, *, #9450, .F. ) ;
#14226 = EDGE_CURVE ( 'NONE', #3128, #6593, #1329, .T. ) ;
#14227 = ORIENTED_EDGE ( 'NONE', *, *, #3698, .F. ) ;
#14228 = DIRECTION ( 'NONE',  ( 1.000000000000000000, 0.000000000000000000, 1.445602896647339903E-16 ) ) ;
#14229 = DIRECTION ( 'NONE',  ( 0.8660254037844385966, 0.000000000000000000, -0.4999999999999998890 ) ) ;
#14230 = CARTESIAN_POINT ( 'NONE',  ( -1.929411732541991720, -2.859457149331156689, 0.1546924827060817687 ) ) ;
#14231 = CARTESIAN_POINT ( 'NONE',  ( -1.006462590703987470, 36.23251143493319404, 0.4787949826583631774 ) ) ;
#14232 = CARTESIAN_POINT ( 'NONE',  ( 0.000000000000000000, -0.4921259842519685179, 0.000000000000000000 ) ) ;
#14233 = AXIS2_PLACEMENT_3D ( 'NONE', #1433, #7521, #9810 ) ;
#14234 = CARTESIAN_POINT ( 'NONE',  ( -1.579560458409178914, 0.1027931408841043642, -0.07190451969745018101 ) ) ;
#14235 = CARTESIAN_POINT ( 'NONE',  ( -1.391807345368153870, -0.02266535781586121248, 0.03937007891299400264 ) ) ;
#14236 = DIRECTION ( 'NONE',  ( 0.000000000000000000, 0.000000000000000000, 1.000000000000000000 ) ) ;
#14237 = DIRECTION ( 'NONE',  ( -0.4005670834070305664, -0.9162674345903522033, -0.000000000000000000 ) ) ;
#14238 = VERTEX_POINT ( 'NONE', #3762 ) ;
#14239 = EDGE_LOOP ( 'NONE', ( #9097, #5932, #9262, #9170 ) ) ;
#14240 = VERTEX_POINT ( 'NONE', #13306 ) ;
#14241 = ORIENTED_EDGE ( 'NONE', *, *, #12680, .T. ) ;
#14242 = ADVANCED_FACE ( 'NONE', ( #15446 ), #2570, .F. ) ;
#14243 = ADVANCED_FACE ( 'NONE', ( #14566 ), #10023, .F. ) ;
#14244 = DIRECTION ( 'NONE',  ( -1.000000000000000000, 0.000000000000000000, 0.000000000000000000 ) ) ;
#14245 = CARTESIAN_POINT ( 'NONE',  ( -0.02479723250354462505, 0.1726834024554401437, -0.005447726382807938084 ) ) ;
#14246 = EDGE_CURVE ( 'NONE', #8823, #3814, #14742, .T. ) ;
#14247 = CARTESIAN_POINT ( 'NONE',  ( -1.137795275590550936, 0.000000000000000000, 0.02559055118110236185 ) ) ;
#14248 = CARTESIAN_POINT ( 'NONE',  ( -1.580259682937487753, 0.1018956540318995824, -0.04477369844321314740 ) ) ;
#14249 = DIRECTION ( 'NONE',  ( -1.000000000000000000, 0.000000000000000000, 0.000000000000000000 ) ) ;
#14250 = ORIENTED_EDGE ( 'NONE', *, *, #6322, .F. ) ;
#14251 = CARTESIAN_POINT ( 'NONE',  ( 0.000000000000000000, -1.707404996040164512E-17, 0.000000000000000000 ) ) ;
#14252 = DIRECTION ( 'NONE',  ( -0.4999999999999981681, 0.000000000000000000, -0.8660254037844397068 ) ) ;
#14253 = FACE_OUTER_BOUND ( 'NONE', #4697, .T. ) ;
#14254 = ORIENTED_EDGE ( 'NONE', *, *, #6840, .T. ) ;
#14255 = ORIENTED_EDGE ( 'NONE', *, *, #6268, .F. ) ;
#14256 = EDGE_LOOP ( 'NONE', ( #1727, #8456 ) ) ;
#14257 = CARTESIAN_POINT ( 'NONE',  ( -1.992382107315058271, -2.749515453455440905, 0.1756903148397124803 ) ) ;
#14258 = DIRECTION ( 'NONE',  ( 0.5984233124757303290, 0.8011800915434521553, -0.000000000000000000 ) ) ;
#14259 = LINE ( 'NONE', #9491, #7862 ) ;
#14260 = EDGE_CURVE ( 'NONE', #9440, #15416, #5229, .T. ) ;
#14261 = DIRECTION ( 'NONE',  ( 1.224646799147343593E-16, 0.000000000000000000, -1.000000000000000000 ) ) ;
#14262 = DIRECTION ( 'NONE',  ( 0.000000000000000000, 0.000000000000000000, -1.000000000000000000 ) ) ;
#14263 = SPHERICAL_SURFACE ( 'NONE', #10713, 0.003937007874015747977 ) ;
#14264 = CARTESIAN_POINT ( 'NONE',  ( -1.181096721277146377, 0.3434326092093292204, -0.03937007874014959025 ) ) ;
#14265 = EDGE_LOOP ( 'NONE', ( #328, #10342, #2052, #9282, #10150, #7402, #7346 ) ) ;
#14266 = CARTESIAN_POINT ( 'NONE',  ( -1.995625621700811925, -2.802058942328566893, 0.1561600152793889418 ) ) ;
#14267 = CARTESIAN_POINT ( 'NONE',  ( 0.000000000000000000, -0.4881889763779528324, 0.000000000000000000 ) ) ;
#14268 = LINE ( 'NONE', #8304, #6696 ) ;
#14269 = CARTESIAN_POINT ( 'NONE',  ( -0.5418660417173573052, -0.4881889763779528324, 0.2355633981508970520 ) ) ;
#14270 = ORIENTED_EDGE ( 'NONE', *, *, #3763, .F. ) ;
#14271 = ORIENTED_EDGE ( 'NONE', *, *, #13916, .T. ) ;
#14272 = ORIENTED_EDGE ( 'NONE', *, *, #7374, .T. ) ;
#14273 = DIRECTION ( 'NONE',  ( -1.000000000000000000, -0.000000000000000000, 8.673617379884087537E-15 ) ) ;
#14274 = FACE_OUTER_BOUND ( 'NONE', #337, .T. ) ;
#14275 = LINE ( 'NONE', #11534, #5892 ) ;
#14276 = CARTESIAN_POINT ( 'NONE',  ( -1.403183357138765963, -0.03069084635762514210, 0.04402914006448389178 ) ) ;
#14277 = CARTESIAN_POINT ( 'NONE',  ( 4.821444091131311524E-18, 0.1692468441617604180, 0.03937007874015747977 ) ) ;
#14278 = ITEM_DEFINED_TRANSFORMATION ( 'NONE', 'NONE', #8870,  #11481 ) ;
#14279 = DIRECTION ( 'NONE',  ( 1.000000000000000000, -0.000000000000000000, 0.000000000000000000 ) ) ;
#14280 = ADVANCED_FACE ( 'NONE', ( #13539 ), #2801, .F. ) ;
#14281 = FACE_OUTER_BOUND ( 'NONE', #14068, .T. ) ;
#14282 = ORIENTED_EDGE ( 'NONE', *, *, #11953, .T. ) ;
#14283 = CARTESIAN_POINT ( 'NONE',  ( -0.1181102362204723977, 2.444206406002937815, 0.03937007874015747977 ) ) ;
#14284 = DIRECTION ( 'NONE',  ( 0.000000000000000000, 0.000000000000000000, -1.000000000000000000 ) ) ;
#14285 = CARTESIAN_POINT ( 'NONE',  ( 0.09842519685044820443, -0.1023622047244094474, -0.5909884645248143498 ) ) ;
#14286 = EDGE_CURVE ( 'NONE', #5281, #4762, #12942, .T. ) ;
#14287 = DIRECTION ( 'NONE',  ( 0.8660254037844365982, -0.000000000000000000, 0.5000000000000035527 ) ) ;
#14288 = ORIENTED_EDGE ( 'NONE', *, *, #7777, .F. ) ;
#14289 = ORIENTED_EDGE ( 'NONE', *, *, #9263, .T. ) ;
#14290 = ORIENTED_EDGE ( 'NONE', *, *, #14704, .F. ) ;
#14291 = ORIENTED_EDGE ( 'NONE', *, *, #6835, .T. ) ;
#14292 = ORIENTED_EDGE ( 'NONE', *, *, #8122, .T. ) ;
#14293 = DIRECTION ( 'NONE',  ( 1.000000000000000000, -0.000000000000000000, -0.000000000000000000 ) ) ;
#14294 = DIRECTION ( 'NONE',  ( 0.000000000000000000, 0.000000000000000000, 1.000000000000000000 ) ) ;
#14295 = CYLINDRICAL_SURFACE ( 'NONE', #3593, 0.003937007874015750579 ) ;
#14296 = ADVANCED_FACE ( 'NONE', ( #625 ), #6405, .T. ) ;
#14297 = DIRECTION ( 'NONE',  ( -0.4932581959314704667, 0.8219459448134283086, 0.2847827522010265566 ) ) ;
#14298 = DIRECTION ( 'NONE',  ( 3.614007241618347785E-16, -0.000000000000000000, -1.000000000000000000 ) ) ;
#14299 = EDGE_CURVE ( 'NONE', #14592, #697, #5066, .T. ) ;
#14300 = DIRECTION ( 'NONE',  ( 0.000000000000000000, 0.000000000000000000, -1.000000000000000000 ) ) ;
#14301 = DIRECTION ( 'NONE',  ( -0.8660254037844385966, -0.000000000000000000, -0.5000000000000000000 ) ) ;
#14302 = CARTESIAN_POINT ( 'NONE',  ( 0.5595825771504284729, -0.4921259842519685179, 0.2048774586467246028 ) ) ;
#14303 = EDGE_CURVE ( 'NONE', #1695, #11091, #4438, .T. ) ;
#14304 = CARTESIAN_POINT ( 'NONE',  ( -1.403713693041773514, -0.03108975223222291279, 0.04439787872945648306 ) ) ;
#14305 = FACE_OUTER_BOUND ( 'NONE', #14748, .T. ) ;
#14306 = ORIENTED_EDGE ( 'NONE', *, *, #7682, .T. ) ;
#14307 = EDGE_LOOP ( 'NONE', ( #8792, #3788, #68, #5755 ) ) ;
#14308 = ORIENTED_EDGE ( 'NONE', *, *, #9403, .T. ) ;
#14309 = ORIENTED_EDGE ( 'NONE', *, *, #12944, .F. ) ;
#14310 = DIRECTION ( 'NONE',  ( -1.000000000000000000, 2.168404344971007142E-16, 0.000000000000000000 ) ) ;
#14311 = ADVANCED_FACE ( 'NONE', ( #6310 ), #6979, .T. ) ;
#14312 = DIRECTION ( 'NONE',  ( -1.000000000000000000, 0.000000000000000000, 0.000000000000000000 ) ) ;
#14313 = FACE_OUTER_BOUND ( 'NONE', #5725, .T. ) ;
#14314 = DIRECTION ( 'NONE',  ( -0.000000000000000000, 1.000000000000000000, -0.000000000000000000 ) ) ;
#14315 = DIRECTION ( 'NONE',  ( -0.000000000000000000, -0.000000000000000000, -1.000000000000000000 ) ) ;
#14316 = ORIENTED_EDGE ( 'NONE', *, *, #1858, .F. ) ;
#14317 = DIRECTION ( 'NONE',  ( 0.000000000000000000, 0.000000000000000000, -1.000000000000000000 ) ) ;
#14318 = EDGE_CURVE ( 'NONE', #9714, #6660, #6487, .T. ) ;
#14319 = DIRECTION ( 'NONE',  ( 0.000000000000000000, 0.000000000000000000, -1.000000000000000000 ) ) ;
#14320 = CARTESIAN_POINT ( 'NONE',  ( -1.591501945092674841, 0.08600752902535285793, -0.08366141732283460808 ) ) ;
#14321 = EDGE_CURVE ( 'NONE', #9228, #10534, #7191, .T. ) ;
#14322 = EDGE_LOOP ( 'NONE', ( #3084, #5346, #9486, #2651, #7230 ) ) ;
#14323 = ORIENTED_EDGE ( 'NONE', *, *, #15367, .F. ) ;
#14324 = ADVANCED_FACE ( 'NONE', ( #10097 ), #15452, .T. ) ;
#14325 = ORIENTED_EDGE ( 'NONE', *, *, #7896, .T. ) ;
#14326 = DIRECTION ( 'NONE',  ( -0.8660254037844363761, -4.956352788505160310E-16, 0.5000000000000041078 ) ) ;
#14327 = CARTESIAN_POINT ( 'NONE',  ( -1.607606114292111643, 0.09732815221480045631, 0.07874015748031495954 ) ) ;
#14328 = CARTESIAN_POINT ( 'NONE',  ( -1.929310418580271191, -2.937766263536936151, -0.06371700066512400729 ) ) ;
#14329 = DIRECTION ( 'NONE',  ( 1.000000000000000000, -0.000000000000000000, -0.000000000000000000 ) ) ;
#14330 = CARTESIAN_POINT ( 'NONE',  ( -0.05260779769176850140, -0.1848037158363092514, -0.03481219553824698582 ) ) ;
#14331 = CARTESIAN_POINT ( 'NONE',  ( -0.09842519685028333631, -0.2952755905511811330, -0.4624047872104675161 ) ) ;
#14332 = DIRECTION ( 'NONE',  ( 1.000000000000000000, 0.000000000000000000, 0.000000000000000000 ) ) ;
#14333 = CARTESIAN_POINT ( 'NONE',  ( -2.111938395807090529, -2.009781522894384054, 0.1096056828055473470 ) ) ;
#14334 = ORIENTED_EDGE ( 'NONE', *, *, #3280, .F. ) ;
#14335 = CARTESIAN_POINT ( 'NONE',  ( -1.951527508739262728, -2.917036378191013135, -0.07732708326134817012 ) ) ;
#14336 = CARTESIAN_POINT ( 'NONE',  ( -0.06278592661683286835, 1.343094183513035222, -0.5877247716201634553 ) ) ;
#14337 = EDGE_CURVE ( 'NONE', #12501, #8290, #8434, .T. ) ;
#14338 = CARTESIAN_POINT ( 'NONE',  ( 0.5445274672588121812, 1.338626482899105241, 0.2461921031270739857 ) ) ;
#14339 = EDGE_LOOP ( 'NONE', ( #9853, #2652, #1652, #9583 ) ) ;
#14340 = VECTOR ( 'NONE', #3002, 39.37007874015748143 ) ;
#14341 = CIRCLE ( 'NONE', #4824, 0.003937007874015724558 ) ;
#14342 = EDGE_CURVE ( 'NONE', #2312, #11304, #10191, .T. ) ;
#14343 = CIRCLE ( 'NONE', #4083, 0.5905511811023621549 ) ;
#14344 = ORIENTED_EDGE ( 'NONE', *, *, #10213, .T. ) ;
#14345 = LINE ( 'NONE', #8394, #11378 ) ;
#14346 = DIRECTION ( 'NONE',  ( 0.4999999999999922284, -0.000000000000000000, -0.8660254037844431485 ) ) ;
#14347 = CARTESIAN_POINT ( 'NONE',  ( -1.417055254560940947, -0.04218366875896984586, 0.06815127639898536926 ) ) ;
#14348 = CARTESIAN_POINT ( 'NONE',  ( 0.1181102362204724254, 2.448818897637795367, -0.03937007874015747977 ) ) ;
#14349 = DIRECTION ( 'NONE',  ( 5.688234090747695582E-25, 1.000000000000000000, 6.210310043996969398E-13 ) ) ;
#14350 = VECTOR ( 'NONE', #9365, 39.37007874015748143 ) ;
#14351 = CARTESIAN_POINT ( 'NONE',  ( 0.000000000000000000, 1.606299212598425674, 0.000000000000000000 ) ) ;
#14352 = ORIENTED_EDGE ( 'NONE', *, *, #7757, .T. ) ;
#14353 = CARTESIAN_POINT ( 'NONE',  ( -1.602629991056316650, 0.1043896402808425078, -0.05327537141226647288 ) ) ;
#14354 = CIRCLE ( 'NONE', #7837, 0.003937007874015749712 ) ;
#14355 = DIRECTION ( 'NONE',  ( -0.000000000000000000, 1.000000000000000000, -0.000000000000000000 ) ) ;
#14356 = CIRCLE ( 'NONE', #4095, 0.003937007874015750579 ) ;
#14357 = DIRECTION ( 'NONE',  ( -0.5000000000000004441, 0.000000000000000000, 0.8660254037844383745 ) ) ;
#14358 = CARTESIAN_POINT ( 'NONE',  ( -0.07002222008683994803, -0.1674826920712332579, 0.05905511811023622659 ) ) ;
#14359 = DIRECTION ( 'NONE',  ( -0.8660254037844428154, 0.000000000000000000, -0.4999999999999926725 ) ) ;
#14360 = VERTEX_POINT ( 'NONE', #12763 ) ;
#14361 = ORIENTED_EDGE ( 'NONE', *, *, #224, .F. ) ;
#14363 = ORIENTED_EDGE ( 'NONE', *, *, #12836, .T. ) ;
#14362 = AXIS2_PLACEMENT_3D ( 'NONE', #12684, #11571, #10175 ) ;
#14364 = VECTOR ( 'NONE', #2611, 39.37007874015748143 ) ;
#14365 = ORIENTED_EDGE ( 'NONE', *, *, #14416, .F. ) ;
#14366 = VECTOR ( 'NONE', #10109, 39.37007874015748854 ) ;
#14367 = AXIS2_PLACEMENT_3D ( 'NONE', #2665, #12237, #11034 ) ;
#14368 = CARTESIAN_POINT ( 'NONE',  ( 4.580371886574746102E-18, 0.4133858267716535306, -0.03543307086614173179 ) ) ;
#14369 = TOROIDAL_SURFACE ( 'NONE', #3379, 0.05905511811023614333, 0.01968503937007873988 ) ;
#14370 =( NAMED_UNIT ( * ) PLANE_ANGLE_UNIT ( ) SI_UNIT ( $, .RADIAN. ) );
#14371 = CARTESIAN_POINT ( 'NONE',  ( 0.03346456692913316738, -0.4921259842519685179, 0.05796233017454786168 ) ) ;
#14372 = CARTESIAN_POINT ( 'NONE',  ( -1.922849157407968246, -2.878884448036508115, -0.1420113206368266712 ) ) ;
#14373 = DIRECTION ( 'NONE',  ( 2.775557561562891351E-16, 0.5695655044020491165, 0.8219459448134284196 ) ) ;
#14374 = DIRECTION ( 'NONE',  ( 0.8660254037844400399, 0.000000000000000000, -0.4999999999999977240 ) ) ;
#14375 = CARTESIAN_POINT ( 'NONE',  ( -0.06956272065387619774, 0.1654544434110864770, 0.03844121289758908183 ) ) ;
#14376 = DIRECTION ( 'NONE',  ( 0.000000000000000000, 0.000000000000000000, 1.000000000000000000 ) ) ;
#14377 = DIRECTION ( 'NONE',  ( 1.000000000000000000, 0.000000000000000000, 0.000000000000000000 ) ) ;
#14378 = CARTESIAN_POINT ( 'NONE',  ( -1.181102362204724310, 0.000000000000000000, -0.02952755905511811330 ) ) ;
#14379 = CIRCLE ( 'NONE', #10382, 0.003937007874015758385 ) ;
#14380 = VECTOR ( 'NONE', #10016, 39.37007874015748854 ) ;
#14381 = AXIS2_PLACEMENT_3D ( 'NONE', #1001, #5747, #14153 ) ;
#14382 = AXIS2_PLACEMENT_3D ( 'NONE', #6884, #15114, #8146 ) ;
#14383 = AXIS2_PLACEMENT_3D ( 'NONE', #5627, #14022, #12542 ) ;
#14384 = CARTESIAN_POINT ( 'NONE',  ( 0.000000000000000000, 0.007874015748031480341, 0.000000000000000000 ) ) ;
#14385 = DIRECTION ( 'NONE',  ( 0.5000000000000001110, 0.000000000000000000, -0.8660254037844384856 ) ) ;
#14386 = CIRCLE ( 'NONE', #6866, 0.01968503937007871907 ) ;
#14387 = VERTEX_POINT ( 'NONE', #13939 ) ;
#14388 = EDGE_CURVE ( 'NONE', #13891, #11599, #1874, .T. ) ;
#14389 = ORIENTED_EDGE ( 'NONE', *, *, #6563, .F. ) ;
#14390 = ORIENTED_EDGE ( 'NONE', *, *, #3561, .T. ) ;
#14391 = EDGE_CURVE ( 'NONE', #14773, #15003, #6425, .T. ) ;
#14392 = ORIENTED_EDGE ( 'NONE', *, *, #3092, .F. ) ;
#14393 = AXIS2_PLACEMENT_3D ( 'NONE', #8731, #12327, #4179 ) ;
#14394 = TOROIDAL_SURFACE ( 'NONE', #5116, 0.007874015748031495954, 0.003937007874015747977 ) ;
#14395 = AXIS2_PLACEMENT_3D ( 'NONE', #10957, #242, #13004 ) ;
#14396 = EDGE_CURVE ( 'NONE', #7929, #5808, #8692, .T. ) ;
#14397 = DIRECTION ( 'NONE',  ( 0.000000000000000000, 0.000000000000000000, 1.000000000000000000 ) ) ;
#14398 = CARTESIAN_POINT ( 'NONE',  ( 0.000000000000000000, 0.06496062992125986590, 0.000000000000000000 ) ) ;
#14399 = VECTOR ( 'NONE', #4841, 39.37007874015748143 ) ;
#14400 = CARTESIAN_POINT ( 'NONE',  ( -0.2362204724409448231, -0.02638708502139245488, 0.05905511811023622659 ) ) ;
#14401 = DIRECTION ( 'NONE',  ( 0.000000000000000000, 0.000000000000000000, -1.000000000000000000 ) ) ;
#14402 = CARTESIAN_POINT ( 'NONE',  ( 0.06299212598430634080, -0.4881889763779528324, -0.2377126739437405434 ) ) ;
#14403 = CARTESIAN_POINT ( 'NONE',  ( 0.4788739157331329821, -0.09842519685039370636, 0.3446689608323530440 ) ) ;
#14404 = ORIENTED_EDGE ( 'NONE', *, *, #15146, .F. ) ;
#14405 = SURFACE_STYLE_USAGE ( .BOTH. , #7105 ) ;
#14406 = CARTESIAN_POINT ( 'NONE',  ( -2.184126211765464287, -1.693613514254861174, -0.08383392658277005749 ) ) ;
#14407 = CARTESIAN_POINT ( 'NONE',  ( 1.928577636452524610E-17, -0.1023622047244094474, -0.1574803149606299191 ) ) ;
#14408 = AXIS2_PLACEMENT_3D ( 'NONE', #6495, #645, #414 ) ;
#14409 = VECTOR ( 'NONE', #15431, 39.37007874015748143 ) ;
#14410 = CIRCLE ( 'NONE', #7395, 0.003937007874015750579 ) ;
#14411 = ORIENTED_EDGE ( 'NONE', *, *, #13834, .T. ) ;
#14412 = ORIENTED_EDGE ( 'NONE', *, *, #6166, .F. ) ;
#14413 = EDGE_CURVE ( 'NONE', #105, #13903, #12606, .T. ) ;
#14414 = VERTEX_POINT ( 'NONE', #4600 ) ;
#14415 = DIRECTION ( 'NONE',  ( 0.000000000000000000, 1.000000000000000000, 0.000000000000000000 ) ) ;
#14416 = EDGE_CURVE ( 'NONE', #9061, #3536, #5617, .T. ) ;
#14417 = EDGE_CURVE ( 'NONE', #6036, #14128, #13443, .T. ) ;
#14418 = CARTESIAN_POINT ( 'NONE',  ( -1.606548329185377932, 0.09883514492709696841, 0.06506891156472163762 ) ) ;
#14419 = CIRCLE ( 'NONE', #9672, 0.03937007874015751446 ) ;
#14420 = AXIS2_PLACEMENT_3D ( 'NONE', #7782, #13987, #9356 ) ;
#14421 = DIRECTION ( 'NONE',  ( 0.000000000000000000, -1.000000000000000000, 0.000000000000000000 ) ) ;
#14422 = CARTESIAN_POINT ( 'NONE',  ( 0.000000000000000000, 0.3622047244094487306, -0.6692913385826770867 ) ) ;
#14423 = CARTESIAN_POINT ( 'NONE',  ( -1.293236445124221312, 0.1355266887446167634, 0.05905511811023622659 ) ) ;
#14424 = CARTESIAN_POINT ( 'NONE',  ( -0.09842519685028361387, -0.4881889763779528324, -3.421829314686310476E-17 ) ) ;
#14425 = CIRCLE ( 'NONE', #14932, 0.003937007874015780069 ) ;
#14426 = CARTESIAN_POINT ( 'NONE',  ( -1.923189478754104176, -2.809775139800132493, 0.1734120223863747368 ) ) ;
#14427 = VERTEX_POINT ( 'NONE', #3276 ) ;
#14428 = DIRECTION ( 'NONE',  ( -1.000000000000000000, 0.000000000000000000, 0.000000000000000000 ) ) ;
#14429 = PLANE ( 'NONE',  #3360 ) ;
#14430 = CARTESIAN_POINT ( 'NONE',  ( -0.02374036903667607959, 0.1505616924844533355, -0.03732860159234810404 ) ) ;
#14431 = ORIENTED_EDGE ( 'NONE', *, *, #13512, .T. ) ;
#14432 = ORIENTED_EDGE ( 'NONE', *, *, #11371, .F. ) ;
#14433 = AXIS2_PLACEMENT_3D ( 'NONE', #2843, #8092, #11789 ) ;
#14434 = ORIENTED_EDGE ( 'NONE', *, *, #2596, .F. ) ;
#14435 = CIRCLE ( 'NONE', #3436, 0.5590551181102362266 ) ;
#14436 = EDGE_LOOP ( 'NONE', ( #9784, #8993, #11818, #4274 ) ) ;
#14437 = EDGE_CURVE ( 'NONE', #12443, #15072, #8137, .T. ) ;
#14438 = CARTESIAN_POINT ( 'NONE',  ( -0.1743691514447623103, -0.4881889763779528324, 0.1734091183126679758 ) ) ;
#14439 = AXIS2_PLACEMENT_3D ( 'NONE', #11538, #8887, #741 ) ;
#14440 = FACE_OUTER_BOUND ( 'NONE', #2059, .T. ) ;
#14441 = PLANE ( 'NONE',  #9637 ) ;
#14442 = CONTEXT_DEPENDENT_SHAPE_REPRESENTATION ( #7002, #1549 ) ;
#14444 = COLOUR_RGB ( '',0.7921568627450980005, 0.8196078431372548767, 0.9333333333333333481 ) ;
#14443 = CARTESIAN_POINT ( 'NONE',  ( 0.1181102362204724254, 2.440944881889764329, 0.03937007874015747977 ) ) ;
#14445 = DIRECTION ( 'NONE',  ( -0.000000000000000000, 0.000000000000000000, 1.000000000000000000 ) ) ;
#14446 = ORIENTED_EDGE ( 'NONE', *, *, #5954, .F. ) ;
#14447 = CARTESIAN_POINT ( 'NONE',  ( 0.000000000000000000, 1.385826771653543510, 0.7007874015748031260 ) ) ;
#14448 = EDGE_CURVE ( 'NONE', #2464, #14862, #14174, .T. ) ;
#14449 = FACE_OUTER_BOUND ( 'NONE', #9022, .T. ) ;
#14450 = VECTOR ( 'NONE', #9011, 39.37007874015748143 ) ;
#14451 = CARTESIAN_POINT ( 'NONE',  ( -0.2325106836983179548, -0.09842519685039370636, 0.06483101467138333018 ) ) ;
#14452 = FACE_OUTER_BOUND ( 'NONE', #14580, .T. ) ;
#14453 = VERTEX_POINT ( 'NONE', #6717 ) ;
#14454 = VERTEX_POINT ( 'NONE', #9162 ) ;
#14455 = ORIENTED_EDGE ( 'NONE', *, *, #10166, .T. ) ;
#14456 = VECTOR ( 'NONE', #5288, 39.37007874015748143 ) ;
#14457 = EDGE_LOOP ( 'NONE', ( #15056, #488, #11088, #13462 ) ) ;
#14458 = DIRECTION ( 'NONE',  ( 0.000000000000000000, 0.000000000000000000, 1.000000000000000000 ) ) ;
#14459 = CIRCLE ( 'NONE', #1210, 2.194881889763779181 ) ;
#14460 = CARTESIAN_POINT ( 'NONE',  ( -1.293236445124221312, 0.1355266887446167634, 0.03937007874015747977 ) ) ;
#14461 = CARTESIAN_POINT ( 'NONE',  ( -1.591501945092674841, 0.08600752902535294120, -0.07874015748031495954 ) ) ;
#14462 = CARTESIAN_POINT ( 'NONE',  ( 1.149282130984896622, 35.08612325493803041, 0.7999203010508129097 ) ) ;
#14463 = AXIS2_PLACEMENT_3D ( 'NONE', #15465, #1130, #3309 ) ;
#14464 = DIRECTION ( 'NONE',  ( 0.5000000000000037748, -0.000000000000000000, 0.8660254037844365982 ) ) ;
#14465 = DIRECTION ( 'NONE',  ( 1.000000000000000000, -0.000000000000000000, 0.000000000000000000 ) ) ;
#14466 = DIRECTION ( 'NONE',  ( 0.000000000000000000, 0.000000000000000000, -1.000000000000000000 ) ) ;
#14467 = PRODUCT_RELATED_PRODUCT_CATEGORY ( 'part', '', ( #9801 ) ) ;
#14468 = CARTESIAN_POINT ( 'NONE',  ( 0.5418660417173575272, -0.4881889763779528324, 0.2355633981508976627 ) ) ;
#14469 = AXIS2_PLACEMENT_3D ( 'NONE', #7487, #3668, #2638 ) ;
#14470 = DIRECTION ( 'NONE',  ( 0.4999999999999967804, 1.935995467731361712E-14, -0.8660254037844405950 ) ) ;
#14471 = DIRECTION ( 'NONE',  ( -1.224646799147352961E-16, 0.000000000000000000, -1.000000000000000000 ) ) ;
#14472 = AXIS2_PLACEMENT_3D ( 'NONE', #486, #1650, #7576 ) ;
#14473 = ORIENTED_EDGE ( 'NONE', *, *, #1800, .F. ) ;
#14474 = ORIENTED_EDGE ( 'NONE', *, *, #752, .T. ) ;
#14475 = ORIENTED_EDGE ( 'NONE', *, *, #10676, .T. ) ;
#14476 = LINE ( 'NONE', #6149, #835 ) ;
#14477 = DIRECTION ( 'NONE',  ( 0.000000000000000000, 0.000000000000000000, -1.000000000000000000 ) ) ;
#14478 =( GEOMETRIC_REPRESENTATION_CONTEXT ( 3 ) GLOBAL_UNCERTAINTY_ASSIGNED_CONTEXT ( ( #14896 ) ) GLOBAL_UNIT_ASSIGNED_CONTEXT ( ( #9458, #2069, #13912 ) ) REPRESENTATION_CONTEXT ( 'NONE', 'WORKASPACE' ) );
#14479 = DIRECTION ( 'NONE',  ( -0.8660254037844385966, 0.000000000000000000, -0.5000000000000003331 ) ) ;
#14480 = EDGE_CURVE ( 'NONE', #7594, #14202, #11507, .T. ) ;
#14481 = DIRECTION ( 'NONE',  ( 0.000000000000000000, 0.000000000000000000, -1.000000000000000000 ) ) ;
#14482 = DIRECTION ( 'NONE',  ( -1.000000000000000000, -4.292327424963298981E-16, 5.289613918361266480E-33 ) ) ;
#14483 = CARTESIAN_POINT ( 'NONE',  ( -1.527714331928839098, 0.2380340132385416752, -0.03937007874015747977 ) ) ;
#14484 = EDGE_CURVE ( 'NONE', #13509, #105, #2019, .T. ) ;
#14485 = DIRECTION ( 'NONE',  ( 0.8660254037844365982, -0.000000000000000000, 0.5000000000000035527 ) ) ;
#14486 = CARTESIAN_POINT ( 'NONE',  ( 0.5905511811023622659, -0.2952755905511811330, -0.4190977005962939206 ) ) ;
#14487 = CARTESIAN_POINT ( 'NONE',  ( 0.000000000000000000, 0.07874015748031495954, 0.000000000000000000 ) ) ;
#14488 = ORIENTED_EDGE ( 'NONE', *, *, #6002, .T. ) ;
#14489 = EDGE_CURVE ( 'NONE', #15344, #10478, #9196, .T. ) ;
#14490 = ORIENTED_EDGE ( 'NONE', *, *, #8636, .T. ) ;
#14491 = ORIENTED_EDGE ( 'NONE', *, *, #9143, .F. ) ;
#14492 = ORIENTED_EDGE ( 'NONE', *, *, #9169, .F. ) ;
#14493 = DIRECTION ( 'NONE',  ( 0.000000000000000000, 0.000000000000000000, 1.000000000000000000 ) ) ;
#14494 = DIRECTION ( 'NONE',  ( -0.000000000000000000, -0.000000000000000000, -1.000000000000000000 ) ) ;
#14495 = CARTESIAN_POINT ( 'NONE',  ( -0.5424653753748054363, 1.043012296488531332, 0.2450015538227584277 ) ) ;
#14496 = ADVANCED_FACE ( 'NONE', ( #10318 ), #5423, .T. ) ;
#14497 = CARTESIAN_POINT ( 'NONE',  ( -0.5894146648244306119, -0.09842519685039370636, 0.1571437749735178357 ) ) ;
#14498 = FACE_OUTER_BOUND ( 'NONE', #6174, .T. ) ;
#14499 = CARTESIAN_POINT ( 'NONE',  ( -2.030412493207266689, -2.521649992949083874, 0.1490301379651515212 ) ) ;
#14500 = EDGE_CURVE ( 'NONE', #6393, #10256, #6412, .T. ) ;
#14501 = ORIENTED_EDGE ( 'NONE', *, *, #11347, .T. ) ;
#14502 = DIRECTION ( 'NONE',  ( 3.476578583725179813E-16, 0.000000000000000000, -1.000000000000000000 ) ) ;
#14503 = CARTESIAN_POINT ( 'NONE',  ( -0.3964138223131424277, -0.2952755905511811330, 0.1515865201236452631 ) ) ;
#14504 = ORIENTED_EDGE ( 'NONE', *, *, #15420, .T. ) ;
#14505 = ADVANCED_FACE ( 'NONE', ( #15266 ), #5763, .T. ) ;
#14506 = ORIENTED_EDGE ( 'NONE', *, *, #8684, .F. ) ;
#14507 = EDGE_LOOP ( 'NONE', ( #9469, #2710 ) ) ;
#14508 = CARTESIAN_POINT ( 'NONE',  ( -1.527714331928839098, 0.2380340132385416752, 0.05905511811023622659 ) ) ;
#14509 = DIRECTION ( 'NONE',  ( -1.445602896647339903E-16, -0.000000000000000000, 1.000000000000000000 ) ) ;
#14510 =( REPRESENTATION_RELATIONSHIP ('NONE','NONE', #8904, #2403 ) REPRESENTATION_RELATIONSHIP_WITH_TRANSFORMATION ( #3240 )SHAPE_REPRESENTATION_RELATIONSHIP( ) );
#14511 = DIRECTION ( 'NONE',  ( 1.000000000000000000, 0.000000000000000000, 0.000000000000000000 ) ) ;
#14512 = CARTESIAN_POINT ( 'NONE',  ( -1.398495881576244493, -0.02731002314121873387, 0.1968503937007874127 ) ) ;
#14513 = CARTESIAN_POINT ( 'NONE',  ( 0.000000000000000000, 2.161417322834645827, -0.1574803149606299191 ) ) ;
#14514 = CARTESIAN_POINT ( 'NONE',  ( -1.187759231255085313, 0.3304857737014040842, 0.05905511811023624741 ) ) ;
#14515 = ADVANCED_FACE ( 'NONE', ( #15037 ), #9698, .T. ) ;
#14516 = ORIENTED_EDGE ( 'NONE', *, *, #9644, .T. ) ;
#14517 = DIRECTION ( 'NONE',  ( -0.5000000000000008882, 0.000000000000000000, 0.8660254037844380415 ) ) ;
#14518 = DIRECTION ( 'NONE',  ( 0.5750876580239430158, 0.8180917953313895374, 0.000000000000000000 ) ) ;
#14519 = CARTESIAN_POINT ( 'NONE',  ( 0.4307978335858663188, -0.09448818897637796532, 0.4279391777402731800 ) ) ;
#14520 = CARTESIAN_POINT ( 'NONE',  ( -0.02220179245438124935, -0.1805881202044197775, 0.03580963740886420471 ) ) ;
#14521 = EDGE_CURVE ( 'NONE', #8551, #9061, #2934, .T. ) ;
#14522 = LINE ( 'NONE', #8550, #9449 ) ;
#14523 = EDGE_LOOP ( 'NONE', ( #10190, #15009, #2891 ) ) ;
#14524 = ORIENTED_EDGE ( 'NONE', *, *, #1305, .F. ) ;
#14525 = EDGE_LOOP ( 'NONE', ( #9549, #13217, #12284, #12405 ) ) ;
#14526 = EDGE_LOOP ( 'NONE', ( #10913, #11794, #5393, #4261 ) ) ;
#14527 = ADVANCED_FACE ( 'NONE', ( #710 ), #4287, .F. ) ;
#14528 = DIRECTION ( 'NONE',  ( 0.000000000000000000, 1.000000000000000000, 0.000000000000000000 ) ) ;
#14529 = FACE_OUTER_BOUND ( 'NONE', #2825, .T. ) ;
#14530 = CARTESIAN_POINT ( 'NONE',  ( 0.000000000000000000, 1.417322834645669438, 0.000000000000000000 ) ) ;
#14531 = CARTESIAN_POINT ( 'NONE',  ( -1.119754571930595244, 35.08612325493829331, 0.8510635335583035532 ) ) ;
#14532 = CARTESIAN_POINT ( 'NONE',  ( -1.181102362204724310, 0.1240157480314959815, -0.02559055118110236185 ) ) ;
#14533 = DIRECTION ( 'NONE',  ( 0.000000000000000000, 1.000000000000000000, 0.000000000000000000 ) ) ;
#14534 = CARTESIAN_POINT ( 'NONE',  ( 0.4121618538092042816, -0.2952755905511811330, 0.1243101294532687889 ) ) ;
#14535 = DIRECTION ( 'NONE',  ( 0.000000000000000000, 0.000000000000000000, -1.000000000000000000 ) ) ;
#14536 = DIRECTION ( 'NONE',  ( -0.5005078764078491060, -0.7027276007399325675, -0.5056340423784807525 ) ) ;
#14537 = DIRECTION ( 'NONE',  ( 1.000000000000000000, 0.000000000000000000, 0.000000000000000000 ) ) ;
#14538 = ORIENTED_EDGE ( 'NONE', *, *, #1552, .T. ) ;
#14539 = ORIENTED_EDGE ( 'NONE', *, *, #2774, .T. ) ;
#14540 = VERTEX_POINT ( 'NONE', #7033 ) ;
#14541 = EDGE_CURVE ( 'NONE', #5934, #10775, #3517, .T. ) ;
#14542 = CARTESIAN_POINT ( 'NONE',  ( -1.964126537190516331, -2.749515453455444014, -0.1756903148397123138 ) ) ;
#14543 = CARTESIAN_POINT ( 'NONE',  ( -0.6864776960422502849, 1.338582677165354395, 0.4645290592786118222 ) ) ;
#14544 = FACE_OUTER_BOUND ( 'NONE', #2223, .T. ) ;
#14545 = DIRECTION ( 'NONE',  ( 0.000000000000000000, -1.000000000000000000, 0.000000000000000000 ) ) ;
#14546 = CARTESIAN_POINT ( 'NONE',  ( -0.5649606299212329708, -0.1023622047244094474, 0.2034364137499347913 ) ) ;
#14547 = DIRECTION ( 'NONE',  ( 0.9966420383350262924, 0.000000000000000000, 0.08188191145426275408 ) ) ;
#14548 = DIRECTION ( 'NONE',  ( 0.000000000000000000, 0.000000000000000000, -1.000000000000000000 ) ) ;
#14549 = CARTESIAN_POINT ( 'NONE',  ( 0.000000000000000000, 1.622047244094488638, 0.000000000000000000 ) ) ;
#14550 = CARTESIAN_POINT ( 'NONE',  ( 0.000000000000000000, 0.03937007874015749365, 0.000000000000000000 ) ) ;
#14551 = ORIENTED_EDGE ( 'NONE', *, *, #15054, .F. ) ;
#14552 = ORIENTED_EDGE ( 'NONE', *, *, #7960, .T. ) ;
#14553 = ORIENTED_EDGE ( 'NONE', *, *, #8883, .T. ) ;
#14554 = B_SPLINE_CURVE_WITH_KNOTS ( 'NONE', 3,
 ( #15128, #12850, #2208, #7997 ),
 .UNSPECIFIED., .F., .F.,
 ( 4, 4 ),
 ( 0.000000000000000000, 2.119993237936781635E-05 ),
 .UNSPECIFIED. ) ;
#14555 = ORIENTED_EDGE ( 'NONE', *, *, #5872, .F. ) ;
#14556 = VERTEX_POINT ( 'NONE', #10721 ) ;
#14557 = DIRECTION ( 'NONE',  ( 1.000000000000000000, 0.000000000000000000, 0.000000000000000000 ) ) ;
#14558 = DIRECTION ( 'NONE',  ( -0.5000000000000001110, 0.000000000000000000, 0.8660254037844385966 ) ) ;
#14559 = ADVANCED_FACE ( 'NONE', ( #10789 ), #3936, .F. ) ;
#14560 = DIRECTION ( 'NONE',  ( -0.000000000000000000, -1.000000000000000000, -0.000000000000000000 ) ) ;
#14561 = DIRECTION ( 'NONE',  ( -1.224646799147353947E-16, 0.000000000000000000, -1.000000000000000000 ) ) ;
#14562 = CARTESIAN_POINT ( 'NONE',  ( -0.3689582295636769649, -0.2952755905511811885, 0.2857551749459845136 ) ) ;
#14563 = DIRECTION ( 'NONE',  ( 0.000000000000000000, 0.000000000000000000, 1.000000000000000000 ) ) ;
#14564 = CARTESIAN_POINT ( 'NONE',  ( -1.895376452690201940, -2.883359828382185963, -0.1046187747444000948 ) ) ;
#14565 = ORIENTED_EDGE ( 'NONE', *, *, #7868, .T. ) ;
#14566 = FACE_OUTER_BOUND ( 'NONE', #3050, .T. ) ;
#14567 = DIRECTION ( 'NONE',  ( -0.000000000000000000, 0.000000000000000000, -1.000000000000000000 ) ) ;
#14568 = ORIENTED_EDGE ( 'NONE', *, *, #11355, .F. ) ;
#14569 = VERTEX_POINT ( 'NONE', #13145 ) ;
#14570 = EDGE_CURVE ( 'NONE', #426, #7319, #12053, .T. ) ;
#14571 = ORIENTED_EDGE ( 'NONE', *, *, #1743, .T. ) ;
#14572 = EDGE_CURVE ( 'NONE', #8715, #10586, #4691, .T. ) ;
#14573 = DIRECTION ( 'NONE',  ( -0.8660254037844383745, 0.000000000000000000, 0.5000000000000004441 ) ) ;
#14574 = EDGE_CURVE ( 'NONE', #2963, #9161, #14708, .T. ) ;
#14575 = DIRECTION ( 'NONE',  ( -0.000000000000000000, -0.000000000000000000, -1.000000000000000000 ) ) ;
#14576 = PLANE ( 'NONE',  #5091 ) ;
#14577 = CARTESIAN_POINT ( 'NONE',  ( 0.4815353412745612127, 0.000000000000000000, 0.3552976658085785222 ) ) ;
#14578 = DIRECTION ( 'NONE',  ( -0.000000000000000000, -1.000000000000000000, -0.000000000000000000 ) ) ;
#14579 = CARTESIAN_POINT ( 'NONE',  ( -0.05074681685833758865, -0.1845569960845552526, -0.03403827111684314816 ) ) ;
#14580 = EDGE_LOOP ( 'NONE', ( #6927, #1882, #8210, #9103 ) ) ;
#14581 = DIRECTION ( 'NONE',  ( -0.8660254037844385966, 0.000000000000000000, 0.5000000000000001110 ) ) ;
#14582 = CARTESIAN_POINT ( 'NONE',  ( -0.05823215749475443154, 0.06963377358823460983, 0.06105365336398917153 ) ) ;
#14583 = DIRECTION ( 'NONE',  ( 0.000000000000000000, -0.000000000000000000, 1.000000000000000000 ) ) ;
#14584 = AXIS2_PLACEMENT_3D ( 'NONE', #11987, #1246, #5998 ) ;
#14585 = CARTESIAN_POINT ( 'NONE',  ( 0.09842519685044817668, -0.2952755905511811330, -0.4624047872104674606 ) ) ;
#14586 = AXIS2_PLACEMENT_3D ( 'NONE', #4508, #10544, #4583 ) ;
#14587 =( NAMED_UNIT ( * ) SI_UNIT ( $, .STERADIAN. ) SOLID_ANGLE_UNIT ( ) );
#14588 = CIRCLE ( 'NONE', #10584, 0.01968503937007875723 ) ;
#14589 = ORIENTED_EDGE ( 'NONE', *, *, #4098, .T. ) ;
#14590 = ADVANCED_FACE ( 'NONE', ( #4763 ), #5928, .F. ) ;
#14591 = ORIENTED_EDGE ( 'NONE', *, *, #9503, .F. ) ;
#14592 = VERTEX_POINT ( 'NONE', #15429 ) ;
#14593 = EDGE_CURVE ( 'NONE', #6490, #6371, #3190, .T. ) ;
#14594 = VERTEX_POINT ( 'NONE', #2552 ) ;
#14595 = DIRECTION ( 'NONE',  ( 0.000000000000000000, 0.000000000000000000, -1.000000000000000000 ) ) ;
#14596 = CARTESIAN_POINT ( 'NONE',  ( 0.5576140732134206024, -0.4921259842519685179, 0.2082870074805215910 ) ) ;
#14597 = VECTOR ( 'NONE', #4860, 39.37007874015748143 ) ;
#14598 = CIRCLE ( 'NONE', #15095, 0.003937007874015724558 ) ;
#14599 = AXIS2_PLACEMENT_3D ( 'NONE', #10041, #14470, #13351 ) ;
#14600 = ADVANCED_FACE ( 'NONE', ( #4694 ), #15190, .F. ) ;
#14601 = CARTESIAN_POINT ( 'NONE',  ( -1.993158829383584019, -2.659208322459291285, 0.1643215684482012828 ) ) ;
#14602 = CARTESIAN_POINT ( 'NONE',  ( 0.5860051159906327634, 0.000000000000000000, 0.1591122789105294533 ) ) ;
#14603 = AXIS2_PLACEMENT_3D ( 'NONE', #6566, #14908, #15212 ) ;
#14604 = CARTESIAN_POINT ( 'NONE',  ( -0.2033807805266766300, 35.67284691056102730, 0.1174219483851045298 ) ) ;
#14605 = EDGE_CURVE ( 'NONE', #12616, #5966, #12453, .T. ) ;
#14606 = DIRECTION ( 'NONE',  ( -0.000000000000000000, -1.000000000000000000, -0.000000000000000000 ) ) ;
#14607 = FACE_OUTER_BOUND ( 'NONE', #1194, .T. ) ;
#14608 = LINE ( 'NONE', #2617, #7912 ) ;
#14609 = DIRECTION ( 'NONE',  ( -3.973232667114494807E-16, 0.000000000000000000, 1.000000000000000000 ) ) ;
#14610 = CARTESIAN_POINT ( 'NONE',  ( -0.1023622047242992716, -0.4921259842519685179, -0.2472069366677729363 ) ) ;
#14611 = MANIFOLD_SOLID_BREP ( 'Fillet1', #13381 ) ;
#14612 = CARTESIAN_POINT ( 'NONE',  ( 0.5576140732134206024, -0.1023622047244094474, 0.2082870074805215910 ) ) ;
#14613 = AXIS2_PLACEMENT_3D ( 'NONE', #7545, #5439, #10233 ) ;
#14614 = CIRCLE ( 'NONE', #14104, 0.04330708661417326938 ) ;
#14615 = ORIENTED_EDGE ( 'NONE', *, *, #1238, .T. ) ;
#14616 = AXIS2_PLACEMENT_3D ( 'NONE', #4889, #14464, #6935 ) ;
#14617 = AXIS2_PLACEMENT_3D ( 'NONE', #88, #11930, #14102 ) ;
#14618 = ORIENTED_EDGE ( 'NONE', *, *, #1110, .T. ) ;
#14619 = ORIENTED_EDGE ( 'NONE', *, *, #6972, .T. ) ;
#14620 = DIRECTION ( 'NONE',  ( 1.000000000000000000, 0.000000000000000000, 0.000000000000000000 ) ) ;
#14621 = CARTESIAN_POINT ( 'NONE',  ( -1.927720146670603762, -2.942124612819895901, 0.05098125556452735158 ) ) ;
#14622 = CARTESIAN_POINT ( 'NONE',  ( 0.4749369078591172411, -0.4881889763779528324, 0.3514880584999470203 ) ) ;
#14623 = EDGE_CURVE ( 'NONE', #3165, #8556, #11205, .T. ) ;
#14624 = AXIS2_PLACEMENT_3D ( 'NONE', #7566, #14494, #11100 ) ;
#14625 = TOROIDAL_SURFACE ( 'NONE', #8113, 0.1653543307086614012, 0.007874015748031495954 ) ;
#14626 = DIRECTION ( 'NONE',  ( 6.667973881468103839E-14, 9.362029067655382729E-14, -1.000000000000000000 ) ) ;
#14627 = AXIS2_PLACEMENT_3D ( 'NONE', #14979, #9173, #7752 ) ;
#14628 = DIRECTION ( 'NONE',  ( 0.8660254037844385966, 0.000000000000000000, 0.5000000000000000000 ) ) ;
#14629 = AXIS2_PLACEMENT_3D ( 'NONE', #5748, #9535, #15412 ) ;
#14630 = CARTESIAN_POINT ( 'NONE',  ( -0.1531294576120625917, -0.4921259842519685179, -0.08840933357318583874 ) ) ;
#14631 = TOROIDAL_SURFACE ( 'NONE', #7865, 2.814960629921260171, 0.01968503937007873988 ) ;
#14632 = LINE ( 'NONE', #6289, #10652 ) ;
#14633 = EDGE_CURVE ( 'NONE', #15414, #4395, #7643, .T. ) ;
#14634 = PLANE ( 'NONE',  #4449 ) ;
#14635 = CARTESIAN_POINT ( 'NONE',  ( -1.930582750161468297, -2.789131037002329006, 0.1561188479113173599 ) ) ;
#14636 = ADVANCED_FACE ( 'NONE', ( #7553 ), #5182, .T. ) ;
#14637 = DIRECTION ( 'NONE',  ( -0.000000000000000000, -0.000000000000000000, -1.000000000000000000 ) ) ;
#14638 = CARTESIAN_POINT ( 'NONE',  ( 0.6864776960422569463, 1.190944881889763884, 0.4645290592786023298 ) ) ;
#14639 = ORIENTED_EDGE ( 'NONE', *, *, #13330, .T. ) ;
#14640 = ORIENTED_EDGE ( 'NONE', *, *, #14118, .F. ) ;
#14641 = AXIS2_PLACEMENT_3D ( 'NONE', #9989, #6442, #3007 ) ;
#14642 = ORIENTED_EDGE ( 'NONE', *, *, #14541, .T. ) ;
#14643 = AXIS2_PLACEMENT_3D ( 'NONE', #9577, #6258, #8408 ) ;
#14644 = AXIS2_PLACEMENT_3D ( 'NONE', #3283, #15275, #5472 ) ;
#14645 = EDGE_LOOP ( 'NONE', ( #4418, #2759, #3297, #10210, #12570 ) ) ;
#14646 = VERTEX_POINT ( 'NONE', #1624 ) ;
#14647 = AXIS2_PLACEMENT_3D ( 'NONE', #4704, #9492, #14261 ) ;
#14648 = CARTESIAN_POINT ( 'NONE',  ( -1.417802900119197629, -0.04287136125579330687, -0.07339284414834101877 ) ) ;
#14649 = DIRECTION ( 'NONE',  ( -0.4999999999999817368, -0.000000000000000000, -0.8660254037844491437 ) ) ;
#14650 = CARTESIAN_POINT ( 'NONE',  ( 0.09842519685044796851, -0.4881889763779528324, 3.910662073933746312E-17 ) ) ;
#14651 = FACE_OUTER_BOUND ( 'NONE', #13133, .T. ) ;
#14652 = CIRCLE ( 'NONE', #8637, 0.01968503937007875723 ) ;
#14653 = CARTESIAN_POINT ( 'NONE',  ( 1.181102362204724310, -0.1240157480314959815, 0.02952755905511811330 ) ) ;
#14654 = TOROIDAL_SURFACE ( 'NONE', #12907, 0.007874015748031495954, 0.003937007874015747977 ) ;
#14655 = CARTESIAN_POINT ( 'NONE',  ( -1.899925859588517341, -2.943879019075679615, -0.04472015565144684540 ) ) ;
#14656 = AXIS2_PLACEMENT_3D ( 'NONE', #5374, #13386, #3909 ) ;
#14657 = ORIENTED_EDGE ( 'NONE', *, *, #10564, .T. ) ;
#14658 = PRODUCT_RELATED_PRODUCT_CATEGORY ( 'part', '', ( #5029 ) ) ;
#14659 = CARTESIAN_POINT ( 'NONE',  ( 0.000000000000000000, 1.035433070866142113, 0.000000000000000000 ) ) ;
#14660 = VECTOR ( 'NONE', #5461, 39.37007874015748854 ) ;
#14661 = DIRECTION ( 'NONE',  ( 0.000000000000000000, 0.000000000000000000, 1.000000000000000000 ) ) ;
#14662 = ORIENTED_EDGE ( 'NONE', *, *, #5013, .F. ) ;
#14663 = VERTEX_POINT ( 'NONE', #3811 ) ;
#14665 = EDGE_LOOP ( 'NONE', ( #9800, #3567, #3504, #903 ) ) ;
#14664 = CIRCLE ( 'NONE', #3900, 0.6692913385826770867 ) ;
#14666 = CIRCLE ( 'NONE', #1412, 0.01968503937007867396 ) ;
#14667 = AXIS2_PLACEMENT_3D ( 'NONE', #3159, #2927, #7703 ) ;
#14668 = VECTOR ( 'NONE', #50, 39.37007874015748143 ) ;
#14669 = CARTESIAN_POINT ( 'NONE',  ( -1.945459748359985142, -2.745801194614594820, -0.1561691687464109024 ) ) ;
#14670 = CARTESIAN_POINT ( 'NONE',  ( 1.928577636452524610E-17, 0.000000000000000000, 0.1574803149606299191 ) ) ;
#14671 = FACE_OUTER_BOUND ( 'NONE', #14212, .T. ) ;
#14672 = DIRECTION ( 'NONE',  ( 1.000000000000000000, -1.349229370204184369E-15, 0.000000000000000000 ) ) ;
#14673 = DIRECTION ( 'NONE',  ( -0.000000000000000000, 1.000000000000000000, -0.000000000000000000 ) ) ;
#14674 = ORIENTED_EDGE ( 'NONE', *, *, #10484, .F. ) ;
#14675 = EDGE_CURVE ( 'NONE', #9296, #4567, #14459, .T. ) ;
#14676 = DIRECTION ( 'NONE',  ( 0.000000000000000000, 0.000000000000000000, -1.000000000000000000 ) ) ;
#14677 = DIRECTION ( 'NONE',  ( 0.4999999999999979461, 0.000000000000000000, 0.8660254037844398178 ) ) ;
#14678 = CARTESIAN_POINT ( 'NONE',  ( 2.025006518275150778E-17, 0.03149606299212599769, 0.1653543307086614012 ) ) ;
#14679 = COLOUR_RGB ( '',0.7921568627450980005, 0.8196078431372548767, 0.9333333333333333481 ) ;
#14680 = PLANE ( 'NONE',  #15202 ) ;
#14681 = EDGE_CURVE ( 'NONE', #10896, #4883, #10944, .T. ) ;
#14682 = FACE_OUTER_BOUND ( 'NONE', #14867, .T. ) ;
#14683 = AXIS2_PLACEMENT_3D ( 'NONE', #3166, #6357, #8086 ) ;
#14684 = ORIENTED_EDGE ( 'NONE', *, *, #2072, .T. ) ;
#14685 = EDGE_CURVE ( 'NONE', #7280, #9606, #12710, .T. ) ;
#14686 = ORIENTED_EDGE ( 'NONE', *, *, #1501, .F. ) ;
#14687 = VERTEX_POINT ( 'NONE', #12437 ) ;
#14688 = CARTESIAN_POINT ( 'NONE',  ( 0.1724006475077543565, -0.4881889763779528324, 0.1768186671464649640 ) ) ;
#14689 = CARTESIAN_POINT ( 'NONE',  ( 0.000000000000000000, -0.4881889763779528324, 0.1574803149606299191 ) ) ;
#14690 = AXIS2_PLACEMENT_3D ( 'NONE', #12024, #10821, #8489 ) ;
#14691 = CARTESIAN_POINT ( 'NONE',  ( -2.000227613418059214, -2.562930154573033636, 0.1533876257101599305 ) ) ;
#14692 = DIRECTION ( 'NONE',  ( 0.000000000000000000, 0.000000000000000000, -1.000000000000000000 ) ) ;
#14693 = CARTESIAN_POINT ( 'NONE',  ( 0.2033807805269695623, 35.67284691056339341, 0.1174219483852173285 ) ) ;
#14694 = CARTESIAN_POINT ( 'NONE',  ( -1.419615703680148000, -0.01226548409420233701, 0.07587259468772762638 ) ) ;
#14695 = DIRECTION ( 'NONE',  ( 0.000000000000000000, 0.000000000000000000, -1.000000000000000000 ) ) ;
#14696 = CARTESIAN_POINT ( 'NONE',  ( -0.2952755905511810219, -0.02638708502139244100, 0.05905511811023622659 ) ) ;
#14697 = DIRECTION ( 'NONE',  ( 0.8660254037844384856, 0.000000000000000000, 0.5000000000000003331 ) ) ;
#14698 = DIRECTION ( 'NONE',  ( 0.000000000000000000, 0.000000000000000000, -1.000000000000000000 ) ) ;
#14699 = ADVANCED_FACE ( 'NONE', ( #6466 ), #5570, .F. ) ;
#14700 = FACE_OUTER_BOUND ( 'NONE', #13310, .T. ) ;
#14701 = ORIENTED_EDGE ( 'NONE', *, *, #9789, .T. ) ;
#14702 = VECTOR ( 'NONE', #9154, 39.37007874015748143 ) ;
#14703 = ORIENTED_EDGE ( 'NONE', *, *, #11123, .T. ) ;
#14704 = EDGE_CURVE ( 'NONE', #9168, #15219, #6944, .T. ) ;
#14705 = CARTESIAN_POINT ( 'NONE',  ( -0.06299212598414173636, -0.4881889763779528324, -0.2366577558633980449 ) ) ;
#14706 = ADVANCED_FACE ( 'NONE', ( #7066 ), #4654, .T. ) ;
#14707 = ORIENTED_EDGE ( 'NONE', *, *, #3413, .T. ) ;
#14708 = CIRCLE ( 'NONE', #7939, 0.007874015748031475137 ) ;
#14709 = AXIS2_PLACEMENT_3D ( 'NONE', #3478, #14349, #10682 ) ;
#14710 = DIRECTION ( 'NONE',  ( 8.673617379884028076E-17, 1.000000000000000000, 0.000000000000000000 ) ) ;
#14711 = CARTESIAN_POINT ( 'NONE',  ( -1.945925679626857141, -2.930745767159171233, 0.04531667161755153356 ) ) ;
#14712 = CARTESIAN_POINT ( 'NONE',  ( 0.000000000000000000, 2.637795275590551825, -0.03937007874015747977 ) ) ;
#14713 = CIRCLE ( 'NONE', #3198, 0.003937007874015758385 ) ;
#14714 = DIRECTION ( 'NONE',  ( 1.000000000000000000, 0.000000000000000000, 0.000000000000000000 ) ) ;
#14715 = CARTESIAN_POINT ( 'NONE',  ( -0.4141303577462134844, -0.2952755905511811330, 0.1209005806194722171 ) ) ;
#14716 = CARTESIAN_POINT ( 'NONE',  ( -1.591501945092674175, 0.08600752902535260813, 0.08366141732283462196 ) ) ;
#14717 = COLOUR_RGB ( '',0.7921568627450980005, 0.8196078431372548767, 0.9333333333333333481 ) ;
#14718 = CARTESIAN_POINT ( 'NONE',  ( -1.889966060128447367, -2.896982825862624011, 0.08667069204985511366 ) ) ;
#14719 = DIRECTION ( 'NONE',  ( -0.000000000000000000, -1.000000000000000000, -0.000000000000000000 ) ) ;
#14720 = CARTESIAN_POINT ( 'NONE',  ( 0.000000000000000000, 0.3464566929133857109, 0.000000000000000000 ) ) ;
#14721 = ORIENTED_EDGE ( 'NONE', *, *, #14203, .T. ) ;
#14722 = EDGE_CURVE ( 'NONE', #6576, #5898, #14215, .T. ) ;
#14723 = VERTEX_POINT ( 'NONE', #13030 ) ;
#14724 = EDGE_CURVE ( 'NONE', #2195, #1428, #7692, .T. ) ;
#14725 = AXIS2_PLACEMENT_3D ( 'NONE', #1662, #8543, #14672 ) ;
#14726 = ORIENTED_EDGE ( 'NONE', *, *, #1008, .T. ) ;
#14727 = ORIENTED_EDGE ( 'NONE', *, *, #15076, .F. ) ;
#14728 = MANIFOLD_SOLID_BREP ( 'Split Line1', #2859 ) ;
#14729 = ORIENTED_EDGE ( 'NONE', *, *, #4265, .T. ) ;
#14730 = AXIS2_PLACEMENT_3D ( 'NONE', #547, #3999, #6313 ) ;
#14731 = CARTESIAN_POINT ( 'NONE',  ( 0.1023622047244638761, -0.2952755905511811330, -0.4190977005962941426 ) ) ;
#14732 = ADVANCED_FACE ( 'NONE', ( #12798 ), #14634, .F. ) ;
#14733 = DIRECTION ( 'NONE',  ( 0.000000000000000000, 0.000000000000000000, 1.000000000000000000 ) ) ;
#14734 = CARTESIAN_POINT ( 'NONE',  ( -1.276200637803905691, -0.1988000726501942539, 0.03937007874015747977 ) ) ;
#14735 = CARTESIAN_POINT ( 'NONE',  ( -0.4749369078591176296, -0.4921259842519685179, 0.3514880584999472424 ) ) ;
#14736 = CARTESIAN_POINT ( 'NONE',  ( -2.176528721278613077, -2.014897391720707365, 0.1098265554920595383 ) ) ;
#14738 = CARTESIAN_POINT ( 'NONE',  ( 0.05905511811023621271, 1.043012296488531332, -0.5922895726594219479 ) ) ;
#14737 = CIRCLE ( 'NONE', #11993, 0.003937007874015724558 ) ;
#14739 = ADVANCED_BREP_SHAPE_REPRESENTATION ( '', ( #9754, #11481 ), #9487 ) ;
#14740 = CARTESIAN_POINT ( 'NONE',  ( -1.897872764959702474, -2.949505210859929782, -0.006217786254915346096 ) ) ;
#14741 = ORIENTED_EDGE ( 'NONE', *, *, #7483, .F. ) ;
#14742 = LINE ( 'NONE', #11033, #13693 ) ;
#14743 = CARTESIAN_POINT ( 'NONE',  ( -1.592432191551354848, 0.1184937169706836296, 0.04125010960145494843 ) ) ;
#14744 = DIRECTION ( 'NONE',  ( 1.000000000000000000, 0.000000000000000000, 0.000000000000000000 ) ) ;
#14745 = ORIENTED_EDGE ( 'NONE', *, *, #1053, .F. ) ;
#14746 = VERTEX_POINT ( 'NONE', #9276 ) ;
#14747 = UNCERTAINTY_MEASURE_WITH_UNIT (LENGTH_MEASURE( 1.000000000000000082E-05 ), #9518, 'distance_accuracy_value', 'NONE');
#14748 = EDGE_LOOP ( 'NONE', ( #2297, #5699, #8919, #14865 ) ) ;
#14749 = EDGE_CURVE ( 'NONE', #8826, #12461, #5891, .T. ) ;
#14750 = CARTESIAN_POINT ( 'NONE',  ( 0.000000000000000000, 1.409448818897637956, 0.000000000000000000 ) ) ;
#14751 = DIRECTION ( 'NONE',  ( -0.000000000000000000, 0.000000000000000000, 1.000000000000000000 ) ) ;
#14752 = DIRECTION ( 'NONE',  ( 0.000000000000000000, 1.000000000000000000, -0.000000000000000000 ) ) ;
#14753 = LINE ( 'NONE', #10036, #9646 ) ;
#14754 = ORIENTED_EDGE ( 'NONE', *, *, #15058, .F. ) ;
#14755 = CARTESIAN_POINT ( 'NONE',  ( 0.3478321452968100580, -0.2952755905511811330, 0.3144726105131502858 ) ) ;
#14756 = DIRECTION ( 'NONE',  ( 1.000000000000000000, 0.000000000000000000, 0.000000000000000000 ) ) ;
#14757 = CARTESIAN_POINT ( 'NONE',  ( -0.02345217991005641225, -0.1628325660491150295, 0.03705913340085396912 ) ) ;
#14758 = ORIENTED_EDGE ( 'NONE', *, *, #10367, .F. ) ;
#14759 = EDGE_LOOP ( 'NONE', ( #1354, #5993, #13107, #10521 ) ) ;
#14760 = ORIENTED_EDGE ( 'NONE', *, *, #8925, .T. ) ;
#14761 = CARTESIAN_POINT ( 'NONE',  ( 0.1531294576121448037, -0.4881889763779528324, -0.08840933357323313424 ) ) ;
#14762 = DIRECTION ( 'NONE',  ( 0.000000000000000000, 0.000000000000000000, -1.000000000000000000 ) ) ;
#14763 = EDGE_CURVE ( 'NONE', #2746, #8120, #6920, .T. ) ;
#14764 = CARTESIAN_POINT ( 'NONE',  ( -0.06427269473107563580, 0.1662356183066786008, -0.05825535267941485407 ) ) ;
#14765 = DIRECTION ( 'NONE',  ( -1.000000000000000000, 8.673617379884087537E-15, 0.000000000000000000 ) ) ;
#14766 = CARTESIAN_POINT ( 'NONE',  ( -0.4822834645669303311, -0.1023622047244094474, 0.3466374647693611366 ) ) ;
#14767 = LINE ( 'NONE', #8888, #2373 ) ;
#14768 = DIRECTION ( 'NONE',  ( 0.000000000000000000, 2.602085213965215059E-14, 1.000000000000000000 ) ) ;
#14769 = EDGE_CURVE ( 'NONE', #12161, #9377, #6180, .T. ) ;
#14770 = DIRECTION ( 'NONE',  ( 3.476578583725179813E-16, 0.000000000000000000, -1.000000000000000000 ) ) ;
#14771 = FACE_OUTER_BOUND ( 'NONE', #3493, .T. ) ;
#14772 = CARTESIAN_POINT ( 'NONE',  ( 0.3689582295636777420, -0.2952755905511811330, 0.2857551749459849022 ) ) ;
#14773 = VERTEX_POINT ( 'NONE', #14285 ) ;
#14774 = VERTEX_POINT ( 'NONE', #8320 ) ;
#14775 = VERTEX_POINT ( 'NONE', #7155 ) ;
#14776 = EDGE_CURVE ( 'NONE', #8756, #1083, #701, .T. ) ;
#14777 = ADVANCED_FACE ( 'NONE', ( #1216, #14131 ), #4416, .F. ) ;
#14778 = DIRECTION ( 'NONE',  ( -0.000000000000000000, -1.000000000000000000, -0.000000000000000000 ) ) ;
#14779 = CARTESIAN_POINT ( 'NONE',  ( -1.943213546182679163, -2.937317732503017531, -0.01185211799045717516 ) ) ;
#14780 = LINE ( 'NONE', #6525, #956 ) ;
#14781 = EDGE_CURVE ( 'NONE', #13986, #11669, #2451, .T. ) ;
#14782 = FACE_BOUND ( 'NONE', #8534, .T. ) ;
#14783 = CARTESIAN_POINT ( 'NONE',  ( -1.181102362204724310, 0.000000000000000000, -0.02559055118110236185 ) ) ;
#14784 = FACE_OUTER_BOUND ( 'NONE', #15239, .T. ) ;
#14785 = CARTESIAN_POINT ( 'NONE',  ( -0.004403105188762939347, -0.1701273036488648305, 3.906667514412696694E-16 ) ) ;
#14786 = CARTESIAN_POINT ( 'NONE',  ( -1.992382107315057160, -2.749515453455444014, -0.1756903148397123138 ) ) ;
#14787 = CARTESIAN_POINT ( 'NONE',  ( 1.181102362204724310, 0.1279527559055117225, 0.02559055118110236185 ) ) ;
#14788 = VERTEX_POINT ( 'NONE', #35 ) ;
#14789 = VERTEX_POINT ( 'NONE', #8549 ) ;
#14790 = VERTEX_POINT ( 'NONE', #1576 ) ;
#14791 = VERTEX_POINT ( 'NONE', #12085 ) ;
#14792 = EDGE_CURVE ( 'NONE', #7799, #6857, #1511, .T. ) ;
#14793 = ORIENTED_EDGE ( 'NONE', *, *, #9695, .F. ) ;
#14794 = EDGE_CURVE ( 'NONE', #3678, #7280, #9717, .T. ) ;
#14795 = CYLINDRICAL_SURFACE ( 'NONE', #7627, 0.003937007874015721089 ) ;
#14796 = CARTESIAN_POINT ( 'NONE',  ( -0.09842519685028340570, -0.4881889763779528324, -0.5909884645248143498 ) ) ;
#14797 = DIRECTION ( 'NONE',  ( -0.000000000000000000, -0.000000000000000000, -1.000000000000000000 ) ) ;
#14798 = DIRECTION ( 'NONE',  ( -0.000000000000000000, -0.000000000000000000, 1.000000000000000000 ) ) ;
#14799 = ADVANCED_FACE ( 'NONE', ( #8411 ), #14680, .F. ) ;
#14800 = CARTESIAN_POINT ( 'NONE',  ( 1.181102362204724310, 4.044111181948214319E-16, 0.02559055118110236185 ) ) ;
#14801 = DIRECTION ( 'NONE',  ( -1.000000000000000000, 0.000000000000000000, 0.000000000000000000 ) ) ;
#14802 = CARTESIAN_POINT ( 'NONE',  ( -1.904949078685900909, -2.929982408226253110, 0.08107751447060709826 ) ) ;
#14803 = ORIENTED_EDGE ( 'NONE', *, *, #1427, .F. ) ;
#14804 = DIRECTION ( 'NONE',  ( -0.000000000000000000, -1.000000000000000000, -0.000000000000000000 ) ) ;
#14805 = CARTESIAN_POINT ( 'NONE',  ( -1.190198933766853706, 0.3259758027579612860, -0.05905511811023622659 ) ) ;
#14806 = VERTEX_POINT ( 'NONE', #3633 ) ;
#14807 = EDGE_CURVE ( 'NONE', #14775, #13507, #13958, .T. ) ;
#14808 = ORIENTED_EDGE ( 'NONE', *, *, #13951, .F. ) ;
#14809 = VERTEX_POINT ( 'NONE', #14451 ) ;
#14810 = DIRECTION ( 'NONE',  ( 1.000000000000000000, -0.000000000000000000, -0.000000000000000000 ) ) ;
#14811 = DIRECTION ( 'NONE',  ( 0.000000000000000000, 0.000000000000000000, -1.000000000000000000 ) ) ;
#14812 = EDGE_CURVE ( 'NONE', #2740, #9755, #11455, .T. ) ;
#14813 = CARTESIAN_POINT ( 'NONE',  ( 0.2661821753648509481, -0.09842519685039372024, 0.03548265769547701703 ) ) ;
#14814 = DIRECTION ( 'NONE',  ( 0.000000000000000000, -1.000000000000000000, 0.000000000000000000 ) ) ;
#14815 = DIRECTION ( 'NONE',  ( 1.000000000000000000, 0.000000000000000000, 0.000000000000000000 ) ) ;
#14816 = ORIENTED_EDGE ( 'NONE', *, *, #11368, .T. ) ;
#14817 = DIRECTION ( 'NONE',  ( -0.8660254037844394848, 0.000000000000000000, -0.4999999999999985567 ) ) ;
#14818 = CARTESIAN_POINT ( 'NONE',  ( 0.1734555655881918346, -0.4921259842519685179, 0.1728816592724491952 ) ) ;
#14819 = DIRECTION ( 'NONE',  ( 0.000000000000000000, 1.000000000000000000, 0.000000000000000000 ) ) ;
#14820 = CARTESIAN_POINT ( 'NONE',  ( -0.2393297813659119866, -0.4881889763779528324, 0.06089400679736760302 ) ) ;
#14821 = EDGE_CURVE ( 'NONE', #12320, #2868, #5436, .T. ) ;
#14822 = CARTESIAN_POINT ( 'NONE',  ( -0.5452492930724200937, 1.043307086614173373, 0.2466088494548779875 ) ) ;
#14823 = EDGE_CURVE ( 'NONE', #563, #10886, #15466, .T. ) ;
#14824 = ORIENTED_EDGE ( 'NONE', *, *, #15068, .T. ) ;
#14825 = ORIENTED_EDGE ( 'NONE', *, *, #13721, .T. ) ;
#14826 = VERTEX_POINT ( 'NONE', #2522 ) ;
#14827 = SPHERICAL_SURFACE ( 'NONE', #2655, 0.003937007874015747977 ) ;
#14828 = DIRECTION ( 'NONE',  ( 0.5000000000000035527, 0.000000000000000000, -0.8660254037844365982 ) ) ;
#14829 = FACE_OUTER_BOUND ( 'NONE', #14339, .T. ) ;
#14830 = CARTESIAN_POINT ( 'NONE',  ( -0.4788739157331333707, -0.09448818897637796532, 0.3446689608323532106 ) ) ;
#14831 = CARTESIAN_POINT ( 'NONE',  ( 1.006462590690022418, 36.23251143493367721, 0.4787949826502353456 ) ) ;
#14832 = LINE ( 'NONE', #7309, #15366 ) ;
#14833 = VECTOR ( 'NONE', #7489, 39.37007874015748143 ) ;
#14834 = LINE ( 'NONE', #6356, #10632 ) ;
#14835 = CARTESIAN_POINT ( 'NONE',  ( -2.010991777528384095, -2.758467574604078543, -0.1561691687464109024 ) ) ;
#14836 = DIRECTION ( 'NONE',  ( 0.000000000000000000, 1.000000000000000000, 0.000000000000000000 ) ) ;
#14837 = CARTESIAN_POINT ( 'NONE',  ( 0.3589087851413743646, -0.2952755905511811330, 0.1299329768165582988 ) ) ;
#14838 = FACE_OUTER_BOUND ( 'NONE', #3148, .T. ) ;
#14839 = VERTEX_POINT ( 'NONE', #10988 ) ;
#14840 = DIRECTION ( 'NONE',  ( 0.4999999999999966693, 0.000000000000000000, 0.8660254037844405950 ) ) ;
#14842 = ORIENTED_EDGE ( 'NONE', *, *, #4532, .T. ) ;
#14841 = AXIS2_PLACEMENT_3D ( 'NONE', #15222, #6812, #15294 ) ;
#14843 = AXIS2_PLACEMENT_3D ( 'NONE', #12411, #13498, #14692 ) ;
#14844 = ORIENTED_EDGE ( 'NONE', *, *, #9901, .F. ) ;
#14845 = VECTOR ( 'NONE', #13080, 39.37007874015748854 ) ;
#14846 = AXIS2_PLACEMENT_3D ( 'NONE', #12293, #10881, #4996 ) ;
#14847 = CARTESIAN_POINT ( 'NONE',  ( 1.181102362204724310, 4.044111181948214319E-16, -0.02559055118110236185 ) ) ;
#14848 = CARTESIAN_POINT ( 'NONE',  ( -1.988221238975143690, -2.822304858211031942, 0.1701874367289316903 ) ) ;
#14849 =( NAMED_UNIT ( * ) PLANE_ANGLE_UNIT ( ) SI_UNIT ( $, .RADIAN. ) );
#14850 = DIRECTION ( 'NONE',  ( 5.204170427930430750E-14, 1.000000000000000000, 0.000000000000000000 ) ) ;
#14851 = CARTESIAN_POINT ( 'NONE',  ( -1.991649887250016571, -2.812956183489762285, -0.1538914628651122662 ) ) ;
#14852 = DIRECTION ( 'NONE',  ( 0.000000000000000000, 1.000000000000000000, 0.000000000000000000 ) ) ;
#14853 = CIRCLE ( 'NONE', #10100, 0.04330708661417324162 ) ;
#14854 = DIRECTION ( 'NONE',  ( 0.000000000000000000, -1.000000000000000000, 0.000000000000000000 ) ) ;
#14855 = CARTESIAN_POINT ( 'NONE',  ( -1.904776753227351849, -2.859193012224173991, -0.1268975449324867832 ) ) ;
#14856 = EDGE_CURVE ( 'NONE', #14240, #6005, #14210, .T. ) ;
#14857 = VECTOR ( 'NONE', #6982, 39.37007874015748143 ) ;
#14858 = DIRECTION ( 'NONE',  ( -0.000000000000000000, -1.000000000000000000, -0.000000000000000000 ) ) ;
#14859 = DIRECTION ( 'NONE',  ( 0.000000000000000000, 0.000000000000000000, 1.000000000000000000 ) ) ;
#14860 = CIRCLE ( 'NONE', #2838, 0.03937007874015751446 ) ;
#14861 = ADVANCED_FACE ( 'NONE', ( #9897 ), #13383, .T. ) ;
#14862 = VERTEX_POINT ( 'NONE', #5242 ) ;
#14863 = ORIENTED_EDGE ( 'NONE', *, *, #13893, .T. ) ;
#14864 = ORIENTED_EDGE ( 'NONE', *, *, #6550, .F. ) ;
#14865 = ORIENTED_EDGE ( 'NONE', *, *, #10364, .F. ) ;
#14866 = EDGE_CURVE ( 'NONE', #15338, #12857, #8215, .T. ) ;
#14867 = EDGE_LOOP ( 'NONE', ( #4109, #7907, #9189, #3469 ) ) ;
#14868 = VECTOR ( 'NONE', #3650, 39.37007874015748854 ) ;
#14869 = AXIS2_PLACEMENT_3D ( 'NONE', #9918, #672, #4100 ) ;
#14870 = CARTESIAN_POINT ( 'NONE',  ( -1.399418326858319572, -0.02634099999489962138, -0.07486975863450967550 ) ) ;
#14871 = TOROIDAL_SURFACE ( 'NONE', #13357, 0.04330708661417328326, 0.003937007874015747977 ) ;
#14872 = CARTESIAN_POINT ( 'NONE',  ( 0.09061599198715353243, 0.06736074103232449206, 0.007444810018878659542 ) ) ;
#14873 = AXIS2_PLACEMENT_3D ( 'NONE', #10968, #2572, #3828 ) ;
#14874 = DIRECTION ( 'NONE',  ( 0.8660254037844383745, 0.000000000000000000, -0.5000000000000004441 ) ) ;
#14875 = TOROIDAL_SURFACE ( 'NONE', #3362, 1.885039370078740451, 0.01968503937007873988 ) ;
#14876 = DIRECTION ( 'NONE',  ( -1.000000000000000000, -0.000000000000000000, 1.734723475976802677E-14 ) ) ;
#14877 = AXIS2_PLACEMENT_3D ( 'NONE', #14604, #9764, #5028 ) ;
#14878 = DIRECTION ( 'NONE',  ( -0.000000000000000000, 0.000000000000000000, 1.000000000000000000 ) ) ;
#14879 = CARTESIAN_POINT ( 'NONE',  ( -0.4854723491485721798, 1.338626482899105241, 0.3484785681409913738 ) ) ;
#14880 = DIRECTION ( 'NONE',  ( 0.000000000000000000, 0.000000000000000000, -1.000000000000000000 ) ) ;
#14881 = CARTESIAN_POINT ( 'NONE',  ( -1.181845651245105211, 0.3414517841021337818, 0.04963174987413059014 ) ) ;
#14882 = CARTESIAN_POINT ( 'NONE',  ( -1.881745788400430719, -2.917268413851039188, 0.04011020394780418635 ) ) ;
#14883 = ORIENTED_EDGE ( 'NONE', *, *, #6646, .T. ) ;
#14884 = CARTESIAN_POINT ( 'NONE',  ( -2.182693454834259139, -1.630005269948474389, -0.08366141732283419175 ) ) ;
#14885 = EDGE_CURVE ( 'NONE', #6434, #4737, #7693, .T. ) ;
#14886 = CARTESIAN_POINT ( 'NONE',  ( 0.000000000000000000, 1.606299212598425674, 0.000000000000000000 ) ) ;
#14887 = AXIS2_PLACEMENT_3D ( 'NONE', #11063, #350, #14695 ) ;
#14888 = VECTOR ( 'NONE', #8129, 39.37007874015748143 ) ;
#14889 = AXIS2_PLACEMENT_3D ( 'NONE', #14610, #353, #5114 ) ;
#14890 = EDGE_CURVE ( 'NONE', #11226, #12382, #10446, .T. ) ;
#14891 = CIRCLE ( 'NONE', #7875, 0.5984251968503937480 ) ;
#14892 = ORIENTED_EDGE ( 'NONE', *, *, #12483, .F. ) ;
#14893 = ORIENTED_EDGE ( 'NONE', *, *, #11548, .F. ) ;
#14894 = VECTOR ( 'NONE', #15442, 39.37007874015748143 ) ;
#14895 = EDGE_CURVE ( 'NONE', #4530, #1873, #11133, .T. ) ;
#14896 = UNCERTAINTY_MEASURE_WITH_UNIT (LENGTH_MEASURE( 1.000000000000000082E-05 ), #9458, 'distance_accuracy_value', 'NONE');
#14897 = ORIENTED_EDGE ( 'NONE', *, *, #13784, .T. ) ;
#14898 = CIRCLE ( 'NONE', #1385, 0.003937007874015749712 ) ;
#14899 = AXIS2_PLACEMENT_3D ( 'NONE', #12083, #1281, #2594 ) ;
#14900 = AXIS2_PLACEMENT_3D ( 'NONE', #8105, #7008, #4212 ) ;
#14901 = LINE ( 'NONE', #13639, #3345 ) ;
#14902 =( BOUNDED_SURFACE ( )  B_SPLINE_SURFACE ( 3, 2, ( 
 ( #3914, #12063, #11102 ),
 ( #8527, #13302, #2429 ),
 ( #1325, #245, #8697 ),
 ( #4842, #14736, #8607 ),
 ( #13470, #13391, #7432 ),
 ( #1553, #12148, #2566 ) ),
 .UNSPECIFIED., .F., .F., .T. ) 
 B_SPLINE_SURFACE_WITH_KNOTS ( ( 4, 2, 4 ),
 ( 3, 3 ),
 ( 0.000000000000000000, 0.01443577820670500188, 0.02887155641341000376 ),
 ( 0.000000000000000000, 1.000000000000000000 ),
 .UNSPECIFIED. ) 
 GEOMETRIC_REPRESENTATION_ITEM ( )  RATIONAL_B_SPLINE_SURFACE ( (
 ( 1.000000000000000000, 0.6921057963906867005, 1.000000000000000000),
 ( 1.000000000000000000, 0.6972252234924993797, 1.000000000000000000),
 ( 1.000000000000000000, 0.7010830952492357326, 1.000000000000000000),
 ( 1.000000000000000000, 0.7061401876506447906, 1.000000000000000000),
 ( 1.000000000000000000, 0.7073403273859646401, 1.000000000000000000),
 ( 1.000000000000000000, 0.7071067811865475727, 1.000000000000000000) ) ) 
 REPRESENTATION_ITEM ( '' )  SURFACE ( )  );
#14903 = CYLINDRICAL_SURFACE ( 'NONE', #13127, 0.7086614173228346081 ) ;
#14904 = DIRECTION ( 'NONE',  ( -0.000000000000000000, 1.000000000000000000, -0.000000000000000000 ) ) ;
#14905 = FACE_OUTER_BOUND ( 'NONE', #5301, .T. ) ;
#14906 = ORIENTED_EDGE ( 'NONE', *, *, #529, .F. ) ;
#14907 = CARTESIAN_POINT ( 'NONE',  ( 0.3294846884549027521, -0.2952755905511811330, 0.2675111804726952314 ) ) ;
#14908 = DIRECTION ( 'NONE',  ( -0.000000000000000000, -1.000000000000000000, -0.000000000000000000 ) ) ;
#14909 = CARTESIAN_POINT ( 'NONE',  ( -1.403716511496708508, -0.03109101116648428989, -0.04439443265226927088 ) ) ;
#14910 = DIRECTION ( 'NONE',  ( -0.8660254037844389297, 0.000000000000000000, 0.4999999999999996114 ) ) ;
#14911 =( NAMED_UNIT ( * ) SI_UNIT ( $, .STERADIAN. ) SOLID_ANGLE_UNIT ( ) );
#14912 = CIRCLE ( 'NONE', #13160, 0.1535433070866141780 ) ;
#14913 = VECTOR ( 'NONE', #8049, 39.37007874015748143 ) ;
#14914 = VECTOR ( 'NONE', #13203, 39.37007874015748143 ) ;
#14915 = VERTEX_POINT ( 'NONE', #5407 ) ;
#14916 = EDGE_CURVE ( 'NONE', #5785, #6404, #12398, .T. ) ;
#14917 = ORIENTED_EDGE ( 'NONE', *, *, #1268, .F. ) ;
#14918 = TOROIDAL_SURFACE ( 'NONE', #10660, 0.007874015748031495954, 0.003937007874015747977 ) ;
#14919 = ORIENTED_EDGE ( 'NONE', *, *, #1610, .F. ) ;
#14920 = LINE ( 'NONE', #9034, #4151 ) ;
#14921 = ADVANCED_FACE ( 'NONE', ( #3061 ), #14988, .T. ) ;
#14922 = CARTESIAN_POINT ( 'NONE',  ( -2.058365226014241767, -2.288432112655881756, 0.1082654573574225593 ) ) ;
#14923 = CARTESIAN_POINT ( 'NONE',  ( 0.5860051159906326523, -0.09448818897637796532, 0.1591122789105293422 ) ) ;
#14924 = APPLICATION_PROTOCOL_DEFINITION ( 'draft international standard', 'automotive_design', 1998, #900 ) ;
#14925 = CIRCLE ( 'NONE', #8164, 0.003937007874015737569 ) ;
#14926 = CARTESIAN_POINT ( 'NONE',  ( 6.701807286672523049E-17, 2.401574803149606918, -0.5433070866141731514 ) ) ;
#14927 = CONICAL_SURFACE ( 'NONE', #9407, 0.08858267716535432601, 1.047197551196600074 ) ;
#14928 = DIRECTION ( 'NONE',  ( 0.000000000000000000, 0.000000000000000000, -1.000000000000000000 ) ) ;
#14929 = FACE_OUTER_BOUND ( 'NONE', #9013, .T. ) ;
#14930 = B_SPLINE_CURVE_WITH_KNOTS ( 'NONE', 3,
 ( #3870, #12036, #7394, #13118 ),
 .UNSPECIFIED., .F., .F.,
 ( 4, 4 ),
 ( 0.02666797036717455383, 0.02905127165838908981 ),
 .UNSPECIFIED. ) ;
#14931 = DIRECTION ( 'NONE',  ( -0.4999999999999979461, 0.000000000000000000, -0.8660254037844398178 ) ) ;
#14932 = AXIS2_PLACEMENT_3D ( 'NONE', #15004, #13668, #2936 ) ;
#14933 = DIRECTION ( 'NONE',  ( 1.000000000000000000, 0.000000000000000000, 0.000000000000000000 ) ) ;
#14934 = ORIENTED_EDGE ( 'NONE', *, *, #11031, .T. ) ;
#14935 = VERTEX_POINT ( 'NONE', #9025 ) ;
#14936 = EDGE_LOOP ( 'NONE', ( #12805, #5622, #14516, #13871 ) ) ;
#14937 = VECTOR ( 'NONE', #6448, 39.37007874015748143 ) ;
#14938 = ORIENTED_EDGE ( 'NONE', *, *, #11335, .T. ) ;
#14939 = VECTOR ( 'NONE', #10430, 39.37007874015748143 ) ;
#14940 = FACE_OUTER_BOUND ( 'NONE', #2976, .T. ) ;
#14941 = CARTESIAN_POINT ( 'NONE',  ( -2.007191670727864086, -2.769487694035170922, 0.1575912778707037332 ) ) ;
#14942 = LENGTH_MEASURE_WITH_UNIT ( LENGTH_MEASURE( 0.02539999999999999897 ), #5512 );
#14943 = AXIS2_PLACEMENT_3D ( 'NONE', #6672, #805, #5560 ) ;
#14944 = CARTESIAN_POINT ( 'NONE',  ( 0.4307978335858664853, -0.09448818897637796532, 0.4279391777402732910 ) ) ;
#14945 = FACE_OUTER_BOUND ( 'NONE', #13882, .T. ) ;
#14946 = LINE ( 'NONE', #15019, #7582 ) ;
#14947 = AXIS2_PLACEMENT_3D ( 'NONE', #9099, #7763, #12551 ) ;
#14948 = CARTESIAN_POINT ( 'NONE',  ( 0.000000000000000000, -0.4921259842519685179, 0.000000000000000000 ) ) ;
#14949 = CARTESIAN_POINT ( 'NONE',  ( -2.099922416332452801, -2.385393657770976894, -0.1341751375602835972 ) ) ;
#14950 = FILL_AREA_STYLE_COLOUR ( '', #7154 ) ;
#14951 = VECTOR ( 'NONE', #6874, 39.37007874015748143 ) ;
#14952 = ORIENTED_EDGE ( 'NONE', *, *, #13615, .F. ) ;
#14953 = EDGE_LOOP ( 'NONE', ( #7853, #15413, #15057, #2377 ) ) ;
#14954 = ORIENTED_EDGE ( 'NONE', *, *, #14321, .F. ) ;
#14955 = ORIENTED_EDGE ( 'NONE', *, *, #12193, .T. ) ;
#14956 = VERTEX_POINT ( 'NONE', #9095 ) ;
#14957 = CIRCLE ( 'NONE', #10940, 0.5905511811023621549 ) ;
#14958 = CARTESIAN_POINT ( 'NONE',  ( 0.4854723491485768982, 1.338626482899105241, 0.3484785681409844904 ) ) ;
#14959 = EDGE_CURVE ( 'NONE', #6434, #4728, #7451, .T. ) ;
#14960 = FACE_OUTER_BOUND ( 'NONE', #9132, .T. ) ;
#14961 = CARTESIAN_POINT ( 'NONE',  ( -1.417802900492933782, -0.04287136159519135126, 0.1968503937007874127 ) ) ;
#14962 = EDGE_CURVE ( 'NONE', #9379, #8620, #9976, .T. ) ;
#14963 = DIRECTION ( 'NONE',  ( 0.5000000000000004441, 0.000000000000000000, -0.8660254037844383745 ) ) ;
#14964 = DIRECTION ( 'NONE',  ( 0.000000000000000000, -1.000000000000000000, 0.000000000000000000 ) ) ;
#14965 = CARTESIAN_POINT ( 'NONE',  ( 0.05905511811029059283, -0.1023622047244094474, -0.2366577558633030653 ) ) ;
#14966 = DIRECTION ( 'NONE',  ( -0.000000000000000000, -1.000000000000000000, -0.000000000000000000 ) ) ;
#14967 = CARTESIAN_POINT ( 'NONE',  ( -0.4749369078591176296, -0.4881889763779528324, 0.3514880584999472424 ) ) ;
#14968 = ORIENTED_EDGE ( 'NONE', *, *, #12614, .T. ) ;
#14969 = CARTESIAN_POINT ( 'NONE',  ( 0.000000000000000000, 0.07874015748031495954, 0.000000000000000000 ) ) ;
#14970 = ADVANCED_FACE ( 'NONE', ( #498 ), #10040, .T. ) ;
#14971 = CARTESIAN_POINT ( 'NONE',  ( 0.2681506793018588741, -0.09842519685039370636, 0.03207310886168006359 ) ) ;
#14972 = TOROIDAL_SURFACE ( 'NONE', #4445, 0.6614173228346456046, 0.007874015748031495954 ) ;
#14973 = ORIENTED_EDGE ( 'NONE', *, *, #6234, .F. ) ;
#14974 = VERTEX_POINT ( 'NONE', #4164 ) ;
#14975 = AXIS2_PLACEMENT_3D ( 'NONE', #14503, #3921, #11035 ) ;
#14976 = ORIENTED_EDGE ( 'NONE', *, *, #12193, .F. ) ;
#14977 = EDGE_CURVE ( 'NONE', #14915, #1942, #12306, .T. ) ;
#14978 = ADVANCED_FACE ( 'NONE', ( #5484 ), #10271, .F. ) ;
#14979 = CARTESIAN_POINT ( 'NONE',  ( -1.293236445124221312, 0.1355266887446167634, -0.03937007874015747977 ) ) ;
#14980 = CARTESIAN_POINT ( 'NONE',  ( -0.4815353412745217998, 1.041793866378536437, 0.3474236500605538125 ) ) ;
#14981 = AXIS2_PLACEMENT_3D ( 'NONE', #11983, #1308, #63 ) ;
#14982 = FACE_OUTER_BOUND ( 'NONE', #4276, .T. ) ;
#14983 = DIRECTION ( 'NONE',  ( -0.000000000000000000, -1.000000000000000000, -0.000000000000000000 ) ) ;
#14984 = ORIENTED_EDGE ( 'NONE', *, *, #12702, .T. ) ;
#14985 = DIRECTION ( 'NONE',  ( -0.8660254037844384856, 0.000000000000000000, -0.5000000000000003331 ) ) ;
#14986 = EDGE_CURVE ( 'NONE', #5486, #12971, #14554, .T. ) ;
#14987 = DIRECTION ( 'NONE',  ( 0.000000000000000000, 0.000000000000000000, -1.000000000000000000 ) ) ;
#14988 = SPHERICAL_SURFACE ( 'NONE', #5937, 0.003937007874015747977 ) ;
#14989 = DIRECTION ( 'NONE',  ( 1.224646799147353207E-16, 1.000000000000000000, -0.000000000000000000 ) ) ;
#14990 = ORIENTED_EDGE ( 'NONE', *, *, #10303, .F. ) ;
#14991 = PLANE ( 'NONE',  #8193 ) ;
#14992 = EDGE_LOOP ( 'NONE', ( #11089, #1603, #12043, #14640 ) ) ;
#14993 = ORIENTED_EDGE ( 'NONE', *, *, #14118, .T. ) ;
#14994 =( BOUNDED_SURFACE ( )  B_SPLINE_SURFACE ( 3, 2, ( 
 ( #8318, #1347, #10753 ),
 ( #9575, #9749, #13190 ),
 ( #10816, #6031, #6112 ),
 ( #14353, #8485, #2520 ),
 ( #9670, #13259, #13097 ),
 ( #8546, #13323, #265 ) ),
 .UNSPECIFIED., .F., .F., .T. ) 
 B_SPLINE_SURFACE_WITH_KNOTS ( ( 4, 2, 4 ),
 ( 3, 3 ),
 ( 0.003230360849850198723, 0.003748134328100786311, 0.004265907806351373899 ),
 ( 0.000000000000000000, 1.000000000000000000 ),
 .UNSPECIFIED. ) 
 GEOMETRIC_REPRESENTATION_ITEM ( )  RATIONAL_B_SPLINE_SURFACE ( (
 ( 1.000000000000000000, 0.7048936089935846638, 1.000000000000000000),
 ( 1.000000000000000000, 0.7048811933884949754, 1.000000000000000000),
 ( 1.000000000000000000, 0.7052257929054446262, 1.000000000000000000),
 ( 1.000000000000000000, 0.7061645128344533617, 1.000000000000000000),
 ( 1.000000000000000000, 0.7067576505883527149, 1.000000000000000000),
 ( 1.000000000000000000, 0.7070941911968778859, 1.000000000000000000) ) ) 
 REPRESENTATION_ITEM ( '' )  SURFACE ( )  );
#14995 = DIRECTION ( 'NONE',  ( -1.000000000000000000, -0.000000000000000000, -0.000000000000000000 ) ) ;
#14996 = CARTESIAN_POINT ( 'NONE',  ( -0.7114373258145173518, 1.190944881889763884, 0.3425575548946232507 ) ) ;
#14997 = EDGE_CURVE ( 'NONE', #2079, #9714, #10715, .T. ) ;
#14998 = FACE_OUTER_BOUND ( 'NONE', #9966, .T. ) ;
#14999 = DIRECTION ( 'NONE',  ( 1.000000000000000000, 0.000000000000000000, 0.000000000000000000 ) ) ;
#15000 = APPLICATION_PROTOCOL_DEFINITION ( 'draft international standard', 'automotive_design', 1998, #3292 ) ;
#15001 = LINE ( 'NONE', #12560, #928 ) ;
#15002 = LINE ( 'NONE', #6586, #7872 ) ;
#15003 = VERTEX_POINT ( 'NONE', #11770 ) ;
#15004 = CARTESIAN_POINT ( 'NONE',  ( -0.4552518684890389244, -0.09448818897637796532, 0.3855835468379172903 ) ) ;
#15005 = ADVANCED_FACE ( 'NONE', ( #5783 ), #10575, .T. ) ;
#15006 = DIRECTION ( 'NONE',  ( 0.000000000000000000, 0.000000000000000000, 1.000000000000000000 ) ) ;
#15007 = DIRECTION ( 'NONE',  ( 0.4999999999999922284, -0.000000000000000000, -0.8660254037844431485 ) ) ;
#15008 = DIRECTION ( 'NONE',  ( 0.000000000000000000, 1.000000000000000000, 0.000000000000000000 ) ) ;
#15009 = ORIENTED_EDGE ( 'NONE', *, *, #9530, .T. ) ;
#15010 = ORIENTED_EDGE ( 'NONE', *, *, #2513, .T. ) ;
#15011 = EDGE_CURVE ( 'NONE', #8722, #1546, #11766, .T. ) ;
#15012 = CYLINDRICAL_SURFACE ( 'NONE', #10130, 0.1574803149606299191 ) ;
#15013 = VERTEX_POINT ( 'NONE', #3463 ) ;
#15014 = ORIENTED_EDGE ( 'NONE', *, *, #11903, .F. ) ;
#15015 = CARTESIAN_POINT ( 'NONE',  ( -1.409916934715107484, -0.04334312390809513804, -0.08366141732283458032 ) ) ;
#15016 = CARTESIAN_POINT ( 'NONE',  ( -1.969012519342776324, -2.873039925085861146, 0.1271406377893942174 ) ) ;
#15017 =( REPRESENTATION_RELATIONSHIP ('NONE','NONE', #8904, #11075 ) REPRESENTATION_RELATIONSHIP_WITH_TRANSFORMATION ( #2584 )SHAPE_REPRESENTATION_RELATIONSHIP( ) );
#15018 = CARTESIAN_POINT ( 'NONE',  ( 0.4815353412745266848, 1.041793866378536437, 0.3474236500605469291 ) ) ;
#15019 = CARTESIAN_POINT ( 'NONE',  ( -0.1638199706403874467, -0.09842519685039372024, 0.2127791970528254695 ) ) ;
#15020 = PLANE ( 'NONE',  #9912 ) ;
#15021 = LINE ( 'NONE', #6531, #15340 ) ;
#15022 = CARTESIAN_POINT ( 'NONE',  ( 0.000000000000000000, 0.5590551181102362266, 0.000000000000000000 ) ) ;
#15023 = ORIENTED_EDGE ( 'NONE', *, *, #13928, .F. ) ;
#15024 = ADVANCED_FACE ( 'NONE', ( #12938, #6981 ), #11597, .F. ) ;
#15025 = VERTEX_POINT ( 'NONE', #9181 ) ;
#15026 = EDGE_LOOP ( 'NONE', ( #9657, #14201, #1714, #10868 ) ) ;
#15027 = ORIENTED_EDGE ( 'NONE', *, *, #6655, .F. ) ;
#15028 = FACE_OUTER_BOUND ( 'NONE', #7179, .T. ) ;
#15029 = DIRECTION ( 'NONE',  ( 0.000000000000000000, 0.000000000000000000, -1.000000000000000000 ) ) ;
#15030 = LINE ( 'NONE', #11332, #8953 ) ;
#15031 = CARTESIAN_POINT ( 'NONE',  ( 0.05905511811023622659, 1.338582677165354395, -0.5952259495879738127 ) ) ;
#15032 = FACE_OUTER_BOUND ( 'NONE', #3857, .T. ) ;
#15033 = CARTESIAN_POINT ( 'NONE',  ( 0.000000000000000000, -1.707404996040164512E-17, 0.000000000000000000 ) ) ;
#15034 = DIRECTION ( 'NONE',  ( 0.000000000000000000, -1.000000000000000000, 0.000000000000000000 ) ) ;
#15035 = DIRECTION ( 'NONE',  ( -1.000000000000000000, 0.000000000000000000, 0.000000000000000000 ) ) ;
#15036 = ORIENTED_EDGE ( 'NONE', *, *, #3431, .T. ) ;
#15037 = FACE_OUTER_BOUND ( 'NONE', #3881, .T. ) ;
#15038 = DIRECTION ( 'NONE',  ( 0.000000000000000000, 0.000000000000000000, 1.000000000000000000 ) ) ;
#15039 = EDGE_LOOP ( 'NONE', ( #14474, #5508, #6040, #11129 ) ) ;
#15040 = ORIENTED_EDGE ( 'NONE', *, *, #3227, .F. ) ;
#15041 = ORIENTED_EDGE ( 'NONE', *, *, #1508, .F. ) ;
#15042 = LINE ( 'NONE', #781, #1877 ) ;
#15043 = EDGE_CURVE ( 'NONE', #12332, #14746, #15214, .T. ) ;
#15044 = CARTESIAN_POINT ( 'NONE',  ( -1.431036756819011213, -0.02829858486107873078, -0.08366141732283458032 ) ) ;
#15045 = DIRECTION ( 'NONE',  ( 0.000000000000000000, 0.000000000000000000, -1.000000000000000000 ) ) ;
#15046 = CARTESIAN_POINT ( 'NONE',  ( -0.5576140732134202693, -0.4881889763779528324, 0.2082870074805209248 ) ) ;
#15047 = ORIENTED_EDGE ( 'NONE', *, *, #14417, .T. ) ;
#15048 = CARTESIAN_POINT ( 'NONE',  ( -0.06011003619056348030, -0.1023622047244094474, -0.2337756660698198097 ) ) ;
#15049 = FACE_OUTER_BOUND ( 'NONE', #8168, .T. ) ;
#15050 = CARTESIAN_POINT ( 'NONE',  ( 0.06767366483286080259, -0.2952755905511811330, 0.7209811753676967916 ) ) ;
#15051 = CARTESIAN_POINT ( 'NONE',  ( -1.293236445124221312, 0.1355266887446167634, -0.05905511811023622659 ) ) ;
#15052 = ORIENTED_EDGE ( 'NONE', *, *, #12365, .T. ) ;
#15053 = CYLINDRICAL_SURFACE ( 'NONE', #7676, 8.689140419947479543 ) ;
#15054 = EDGE_CURVE ( 'NONE', #9631, #9959, #5946, .T. ) ;
#15055 = VERTEX_POINT ( 'NONE', #8240 ) ;
#15056 = ORIENTED_EDGE ( 'NONE', *, *, #5315, .T. ) ;
#15057 = ORIENTED_EDGE ( 'NONE', *, *, #4302, .T. ) ;
#15058 = EDGE_CURVE ( 'NONE', #6019, #9541, #3462, .T. ) ;
#15059 = FACE_OUTER_BOUND ( 'NONE', #12940, .T. ) ;
#15060 = PLANE ( 'NONE',  #13153 ) ;
#15061 = DIRECTION ( 'NONE',  ( -0.5801894994542512451, -0.8144815189573213488, 0.000000000000000000 ) ) ;
#15062 = DIRECTION ( 'NONE',  ( 0.000000000000000000, 0.000000000000000000, -1.000000000000000000 ) ) ;
#15063 = CARTESIAN_POINT ( 'NONE',  ( -1.276200637803905691, -0.1988000726501942539, -0.03937007874015747977 ) ) ;
#15064 = CYLINDRICAL_SURFACE ( 'NONE', #2113, 2.795275590551181466 ) ;
#15065 = ORIENTED_EDGE ( 'NONE', *, *, #11168, .F. ) ;
#15066 = LINE ( 'NONE', #4319, #9677 ) ;
#15067 = CARTESIAN_POINT ( 'NONE',  ( 0.000000000000000000, 0.03937007874015749365, -0.5433070866141731514 ) ) ;
#15068 = EDGE_CURVE ( 'NONE', #14594, #6761, #6450, .T. ) ;
#15069 = CARTESIAN_POINT ( 'NONE',  ( 0.000000000000000000, 0.007874015748031480341, -0.5905511811023621549 ) ) ;
#15070 = ORIENTED_EDGE ( 'NONE', *, *, #12761, .T. ) ;
#15071 = ADVANCED_FACE ( 'NONE', ( #11836 ), #7704, .T. ) ;
#15072 = VERTEX_POINT ( 'NONE', #10433 ) ;
#15073 = DIRECTION ( 'NONE',  ( 0.8660254037844385966, 0.000000000000000000, -0.5000000000000003331 ) ) ;
#15074 = ORIENTED_EDGE ( 'NONE', *, *, #15293, .T. ) ;
#15075 = EDGE_LOOP ( 'NONE', ( #8571, #5121, #10792, #3249 ) ) ;
#15076 = EDGE_CURVE ( 'NONE', #10200, #13856, #9970, .T. ) ;
#15077 = EDGE_CURVE ( 'NONE', #8242, #924, #2954, .T. ) ;
#15078 = CARTESIAN_POINT ( 'NONE',  ( 0.5445274672588121812, 1.043263280880422528, 0.2461921031270739857 ) ) ;
#15079 = CARTESIAN_POINT ( 'NONE',  ( -1.984787441652870577, -2.774072082282616591, 0.1775757135651536422 ) ) ;
#15080 = DIRECTION ( 'NONE',  ( -1.000000000000000000, 8.673617379884029309E-17, 0.000000000000000000 ) ) ;
#15081 = LINE ( 'NONE', #12580, #15349 ) ;
#15082 = CARTESIAN_POINT ( 'NONE',  ( -1.992382107315057160, -2.752050336136266484, -0.1561691687464108746 ) ) ;
#15083 = CARTESIAN_POINT ( 'NONE',  ( -2.024465277823495502, -2.569685212987940837, -0.1523387882505266022 ) ) ;
#15084 = VECTOR ( 'NONE', #3895, 39.37007874015748143 ) ;
#15085 = EDGE_LOOP ( 'NONE', ( #8432, #9117, #5886, #8417 ) ) ;
#15086 = AXIS2_PLACEMENT_3D ( 'NONE', #3029, #9144, #8817 ) ;
#15087 = ORIENTED_EDGE ( 'NONE', *, *, #4046, .T. ) ;
#15088 = VECTOR ( 'NONE', #10177, 39.37007874015748143 ) ;
#15089 = ORIENTED_EDGE ( 'NONE', *, *, #5458, .T. ) ;
#15090 = EDGE_LOOP ( 'NONE', ( #13938, #13294, #6614, #1998 ) ) ;
#15091 = EDGE_CURVE ( 'NONE', #7182, #13179, #14268, .T. ) ;
#15092 = CARTESIAN_POINT ( 'NONE',  ( -0.2661821753646866906, -0.4881889763779528324, 0.03548265769538203052 ) ) ;
#15093 = DIRECTION ( 'NONE',  ( 4.336808689942006692E-15, 0.000000000000000000, -1.000000000000000000 ) ) ;
#15094 = TOROIDAL_SURFACE ( 'NONE', #10325, 0.5590551181102362266, 0.007874015748031495954 ) ;
#15095 = AXIS2_PLACEMENT_3D ( 'NONE', #756, #10237, #4269 ) ;
#15096 = ADVANCED_FACE ( 'NONE', ( #790 ), #1704, .T. ) ;
#15097 = CARTESIAN_POINT ( 'NONE',  ( 0.000000000000000000, 0.3228346456692913757, 0.000000000000000000 ) ) ;
#15098 = FACE_OUTER_BOUND ( 'NONE', #3124, .T. ) ;
#15099 = EDGE_CURVE ( 'NONE', #9161, #4029, #10215, .T. ) ;
#15100 = CYLINDRICAL_SURFACE ( 'NONE', #1391, 0.01968503937007875723 ) ;
#15101 = TOROIDAL_SURFACE ( 'NONE', #7839, 0.5984251968503937480, 0.007874015748031495954 ) ;
#15102 = DIRECTION ( 'NONE',  ( 0.000000000000000000, 0.000000000000000000, -1.000000000000000000 ) ) ;
#15103 = CARTESIAN_POINT ( 'NONE',  ( -1.591501945092674841, 0.08600752902535303834, 0.1968503937007874127 ) ) ;
#15104 = ORIENTED_EDGE ( 'NONE', *, *, #3883, .T. ) ;
#15105 = DIRECTION ( 'NONE',  ( 0.5000000000000041078, -0.000000000000000000, 0.8660254037844363761 ) ) ;
#15106 = CARTESIAN_POINT ( 'NONE',  ( 1.928577636452524610E-17, 2.161417322834645827, 0.1574803149606299191 ) ) ;
#15107 = ORIENTED_EDGE ( 'NONE', *, *, #4515, .F. ) ;
#15108 = EDGE_LOOP ( 'NONE', ( #9314, #41, #807, #2727 ) ) ;
#15109 = AXIS2_PLACEMENT_3D ( 'NONE', #10714, #4111, #12339 ) ;
#15110 = AXIS2_PLACEMENT_3D ( 'NONE', #3556, #12032, #9456 ) ;
#15111 = CIRCLE ( 'NONE', #7596, 2.194881889763779181 ) ;
#15112 = ORIENTED_EDGE ( 'NONE', *, *, #5135, .F. ) ;
#15113 = VECTOR ( 'NONE', #12559, 39.37007874015748143 ) ;
#15114 = DIRECTION ( 'NONE',  ( 0.9040582794047686832, 0.000000000000000000, -0.4274092037376937547 ) ) ;
#15115 = DIRECTION ( 'NONE',  ( 0.8660254037844389297, 0.000000000000000000, -0.4999999999999994449 ) ) ;
#15116 = CARTESIAN_POINT ( 'NONE',  ( -1.981764468582493777, -2.783651129948214731, -0.1771653543307010470 ) ) ;
#15117 = CIRCLE ( 'NONE', #3113, 0.03937007874015747977 ) ;
#15118 = CYLINDRICAL_SURFACE ( 'NONE', #5452, 0.5511811023622046335 ) ;
#15119 = VECTOR ( 'NONE', #12655, 39.37007874015748854 ) ;
#15120 = AXIS2_PLACEMENT_3D ( 'NONE', #11646, #11881, #5852 ) ;
#15121 = DIRECTION ( 'NONE',  ( 0.000000000000000000, 0.000000000000000000, -1.000000000000000000 ) ) ;
#15122 = VECTOR ( 'NONE', #14326, 39.37007874015747433 ) ;
#15123 = ORIENTED_EDGE ( 'NONE', *, *, #14856, .F. ) ;
#15124 = DIRECTION ( 'NONE',  ( -1.000000000000000000, 0.000000000000000000, 0.000000000000000000 ) ) ;
#15125 = AXIS2_PLACEMENT_3D ( 'NONE', #15205, #1887, #6648 ) ;
#15126 = CARTESIAN_POINT ( 'NONE',  ( -1.398495881576244493, -0.02731002314121873387, 0.07874015748031495954 ) ) ;
#15127 = VECTOR ( 'NONE', #6011, 39.37007874015748143 ) ;
#15128 = CARTESIAN_POINT ( 'NONE',  ( -0.05905511811023622659, 1.338626482899105241, -0.5946706712680680518 ) ) ;
#15129 = CARTESIAN_POINT ( 'NONE',  ( 0.5576140732134206024, -0.4881889763779528324, 0.2082870074805215910 ) ) ;
#15130 = DIRECTION ( 'NONE',  ( 0.000000000000000000, -1.000000000000000000, 2.208809394877300528E-16 ) ) ;
#15131 = ORIENTED_EDGE ( 'NONE', *, *, #2238, .T. ) ;
#15132 = CARTESIAN_POINT ( 'NONE',  ( -1.607606114292111199, 0.09732815221480028978, 0.07874015748031495954 ) ) ;
#15133 = ORIENTED_EDGE ( 'NONE', *, *, #6530, .T. ) ;
#15135 = ORIENTED_EDGE ( 'NONE', *, *, #7552, .F. ) ;
#15134 = CIRCLE ( 'NONE', #8874, 0.03937007874015751446 ) ;
#15136 = VECTOR ( 'NONE', #9275, 39.37007874015748143 ) ;
#15137 = ORIENTED_EDGE ( 'NONE', *, *, #11056, .T. ) ;
#15138 = TOROIDAL_SURFACE ( 'NONE', #7141, 0.007874015748031495954, 0.003937007874015747977 ) ;
#15139 = CARTESIAN_POINT ( 'NONE',  ( 0.7052242655755273093, -1.858423098537180129, -0.1033464566929129108 ) ) ;
#15140 = DIRECTION ( 'NONE',  ( 0.000000000000000000, 0.000000000000000000, 1.000000000000000000 ) ) ;
#15141 = CIRCLE ( 'NONE', #883, 0.5590551181102362266 ) ;
#15142 = EDGE_CURVE ( 'NONE', #12889, #3736, #11468, .T. ) ;
#15143 = DIRECTION ( 'NONE',  ( -0.8660254037844381525, 0.000000000000000000, 0.5000000000000006661 ) ) ;
#15144 = CARTESIAN_POINT ( 'NONE',  ( -1.584115185264708625, 0.1296286773226378586, -0.03937007874015747977 ) ) ;
#15145 = DIRECTION ( 'NONE',  ( 0.000000000000000000, -0.000000000000000000, -1.000000000000000000 ) ) ;
#15146 = EDGE_CURVE ( 'NONE', #2098, #3506, #9474, .T. ) ;
#15147 = CARTESIAN_POINT ( 'NONE',  ( 0.7052242655755273093, -1.858423098537180129, 0.1968503937007874127 ) ) ;
#15148 = ORIENTED_EDGE ( 'NONE', *, *, #2530, .T. ) ;
#15149 = DIRECTION ( 'NONE',  ( 0.8660254037844385966, 0.000000000000000000, 0.5000000000000000000 ) ) ;
#15150 = CARTESIAN_POINT ( 'NONE',  ( -0.4462573421471757174, -0.2952755905511811330, 0.1439951688233481186 ) ) ;
#15151 = AXIS2_PLACEMENT_3D ( 'NONE', #8284, #10719, #9478 ) ;
#15152 = AXIS2_PLACEMENT_3D ( 'NONE', #4077, #6876, #9896 ) ;
#15153 =( NAMED_UNIT ( * ) PLANE_ANGLE_UNIT ( ) SI_UNIT ( $, .RADIAN. ) );
#15154 = EDGE_CURVE ( 'NONE', #8643, #11443, #10471, .T. ) ;
#15155 = CARTESIAN_POINT ( 'NONE',  ( -0.4342073824196659437, -0.09842519685039370636, 0.4299076816772786080 ) ) ;
#15156 = VERTEX_POINT ( 'NONE', #8389 ) ;
#15157 = CIRCLE ( 'NONE', #12406, 0.003937007874015758385 ) ;
#15158 = EDGE_LOOP ( 'NONE', ( #1279, #10597, #9625, #3966 ) ) ;
#15159 = DIRECTION ( 'NONE',  ( 0.000000000000000000, 0.000000000000000000, 1.000000000000000000 ) ) ;
#15160 = ORIENTED_EDGE ( 'NONE', *, *, #702, .T. ) ;
#15161 = ORIENTED_EDGE ( 'NONE', *, *, #8267, .F. ) ;
#15162 = AXIS2_PLACEMENT_3D ( 'NONE', #1719, #14649, #13775 ) ;
#15163 = EDGE_CURVE ( 'NONE', #2312, #13241, #11984, .T. ) ;
#15164 = DIRECTION ( 'NONE',  ( -0.000000000000000000, -0.000000000000000000, -1.000000000000000000 ) ) ;
#15165 =( CONVERSION_BASED_UNIT ( 'INCH', #10381 ) LENGTH_UNIT ( ) NAMED_UNIT ( #13065 ) );
#15166 = ADVANCED_FACE ( 'NONE', ( #11931, #10970 ), #3765, .T. ) ;
#15167 = PRODUCT_DEFINITION_SHAPE ( 'NONE', 'NONE',  #15486 ) ;
#15168 = DIRECTION ( 'NONE',  ( 1.000000000000000000, -0.000000000000000000, 1.224646799147353207E-16 ) ) ;
#15169 = CARTESIAN_POINT ( 'NONE',  ( -1.580080891953811628, 0.1020406297922293454, -0.07874015748031495954 ) ) ;
#15170 = CARTESIAN_POINT ( 'NONE',  ( -1.580080891953811628, 0.1020406297922293454, 0.1968503937007874127 ) ) ;
#15171 = DIRECTION ( 'NONE',  ( 0.000000000000000000, 1.000000000000000000, -4.956352788505160310E-16 ) ) ;
#15172 = EDGE_CURVE ( 'NONE', #1922, #5666, #2405, .T. ) ;
#15173 = FACE_OUTER_BOUND ( 'NONE', #287, .T. ) ;
#15174 = FACE_OUTER_BOUND ( 'NONE', #7678, .T. ) ;
#15175 = ADVANCED_FACE ( 'NONE', ( #9734, #1198 ), #2438, .F. ) ;
#15176 = CIRCLE ( 'NONE', #10918, 0.007874015748031516770 ) ;
#15177 = ORIENTED_EDGE ( 'NONE', *, *, #4510, .T. ) ;
#15178 = ORIENTED_EDGE ( 'NONE', *, *, #3717, .F. ) ;
#15179 = ORIENTED_EDGE ( 'NONE', *, *, #12527, .F. ) ;
#15180 = AXIS2_PLACEMENT_3D ( 'NONE', #9178, #12713, #13956 ) ;
#15181 = ORIENTED_EDGE ( 'NONE', *, *, #53, .F. ) ;
#15182 = LINE ( 'NONE', #10635, #10594 ) ;
#15183 = CYLINDRICAL_SURFACE ( 'NONE', #6102, 0.003937007874015724558 ) ;
#15184 = PRESENTATION_LAYER_ASSIGNMENT (  '', '', ( #8431 ) ) ;
#15185 = EDGE_CURVE ( 'NONE', #12201, #4124, #8613, .T. ) ;
#15186 = CARTESIAN_POINT ( 'NONE',  ( -0.05072818602969413060, 0.1683578795566401942, 0.03094016780477576098 ) ) ;
#15187 = CARTESIAN_POINT ( 'NONE',  ( 1.181102362204724310, -0.1240157480314955790, 0.02952755905511811330 ) ) ;
#15188 = CARTESIAN_POINT ( 'NONE',  ( -0.07874015748031543138, -0.1682792322177920907, -0.05905511811023622659 ) ) ;
#15189 = DIRECTION ( 'NONE',  ( -0.000000000000000000, -1.000000000000000000, -0.000000000000000000 ) ) ;
#15190 = TOROIDAL_SURFACE ( 'NONE', #1947, 0.007874015748031495954, 0.003937007874015747977 ) ;
#15191 = CARTESIAN_POINT ( 'NONE',  ( -1.899862746731199259, -2.872024215252888535, -0.1471579868410207437 ) ) ;
#15192 = ORIENTED_EDGE ( 'NONE', *, *, #1675, .F. ) ;
#15193 = DIRECTION ( 'NONE',  ( 0.000000000000000000, 1.000000000000000000, 0.000000000000000000 ) ) ;
#15194 = DIRECTION ( 'NONE',  ( 1.000000000000000000, -0.000000000000000000, 1.224646799147353207E-16 ) ) ;
#15195 = EDGE_CURVE ( 'NONE', #6593, #13559, #13718, .T. ) ;
#15196 = ORIENTED_EDGE ( 'NONE', *, *, #4030, .F. ) ;
#15197 = ORIENTED_EDGE ( 'NONE', *, *, #14219, .F. ) ;
#15198 = CIRCLE ( 'NONE', #10724, 0.5905511811023621549 ) ;
#15199 = VECTOR ( 'NONE', #11570, 39.37007874015748143 ) ;
#15200 = ADVANCED_FACE ( 'NONE', ( #5951 ), #13307, .T. ) ;
#15201 = VERTEX_POINT ( 'NONE', #251 ) ;
#15202 = AXIS2_PLACEMENT_3D ( 'NONE', #2685, #13417, #1351 ) ;
#15203 = DIRECTION ( 'NONE',  ( -0.000000000000000000, -1.000000000000000000, -0.000000000000000000 ) ) ;
#15204 = AXIS2_PLACEMENT_3D ( 'NONE', #2362, #9511, #6994 ) ;
#15205 = CARTESIAN_POINT ( 'NONE',  ( 0.000000000000000000, 1.653543307086614567, 0.000000000000000000 ) ) ;
#15206 = CARTESIAN_POINT ( 'NONE',  ( -1.981764765370718440, -2.783650182701201903, 0.1771653543307413203 ) ) ;
#15208 = AXIS2_PLACEMENT_3D ( 'NONE', #1343, #6108, #9217 ) ;
#15207 = PLANE ( 'NONE',  #11479 ) ;
#15209 = DIRECTION ( 'NONE',  ( -0.000000000000000000, 0.000000000000000000, 1.000000000000000000 ) ) ;
#15210 = ORIENTED_EDGE ( 'NONE', *, *, #14437, .F. ) ;
#15211 = FACE_OUTER_BOUND ( 'NONE', #4186, .T. ) ;
#15212 = DIRECTION ( 'NONE',  ( 0.000000000000000000, 0.000000000000000000, -1.000000000000000000 ) ) ;
#15213 =( GEOMETRIC_REPRESENTATION_CONTEXT ( 3 ) GLOBAL_UNCERTAINTY_ASSIGNED_CONTEXT ( ( #12539 ) ) GLOBAL_UNIT_ASSIGNED_CONTEXT ( ( #2257, #6156, #1314 ) ) REPRESENTATION_CONTEXT ( 'NONE', 'WORKASPACE' ) );
#15214 = LINE ( 'NONE', #4629, #220 ) ;
#15215 = CARTESIAN_POINT ( 'NONE',  ( -1.181342415325333350, 0.3435647566446739520, 0.03937007874015747977 ) ) ;
#15216 = VERTEX_POINT ( 'NONE', #12157 ) ;
#15217 = VERTEX_POINT ( 'NONE', #6018 ) ;
#15218 = EDGE_CURVE ( 'NONE', #796, #4540, #12239, .T. ) ;
#15219 = VERTEX_POINT ( 'NONE', #7279 ) ;
#15220 = CIRCLE ( 'NONE', #9216, 0.6614173228346456046 ) ;
#15221 = EDGE_LOOP ( 'NONE', ( #2123, #5431, #15400, #7718, #11928 ) ) ;
#15222 = CARTESIAN_POINT ( 'NONE',  ( 0.2393297813660762718, -0.4881889763779528324, 0.06089400679746261036 ) ) ;
#15223 = DIRECTION ( 'NONE',  ( 0.000000000000000000, -1.000000000000000000, 0.000000000000000000 ) ) ;
#15224 = VECTOR ( 'NONE', #13400, 39.37007874015747433 ) ;
#15225 = CARTESIAN_POINT ( 'NONE',  ( 0.000000000000000000, 1.645669291338583085, 0.000000000000000000 ) ) ;
#15226 = DIRECTION ( 'NONE',  ( 0.8660254037844433705, 0.000000000000000000, 0.4999999999999918954 ) ) ;
#15227 = CARTESIAN_POINT ( 'NONE',  ( 1.181102362204724310, -0.1240157480314955790, 0.02559055118110236185 ) ) ;
#15228 = CARTESIAN_POINT ( 'NONE',  ( -0.05260779769176852222, -0.1848037158363092514, 0.03481219553824697888 ) ) ;
#15229 = EDGE_LOOP ( 'NONE', ( #3174, #7235, #9858 ) ) ;
#15230 = DIRECTION ( 'NONE',  ( 0.9900370584898828819, 0.1408070410764336311, 9.808509035937714109E-16 ) ) ;
#15231 = DIRECTION ( 'NONE',  ( 0.8660254037844405950, 0.000000000000000000, -0.4999999999999966693 ) ) ;
#15232 = AXIS2_PLACEMENT_3D ( 'NONE', #8299, #6891, #1028 ) ;
#15233 = DIRECTION ( 'NONE',  ( 0.8660254037844383745, -0.000000000000000000, 0.5000000000000002220 ) ) ;
#15234 = VERTEX_POINT ( 'NONE', #6245 ) ;
#15235 = VERTEX_POINT ( 'NONE', #10804 ) ;
#15236 = DIRECTION ( 'NONE',  ( -0.000000000000000000, 0.000000000000000000, 1.000000000000000000 ) ) ;
#15237 = ORIENTED_EDGE ( 'NONE', *, *, #12012, .F. ) ;
#15238 = EDGE_CURVE ( 'NONE', #6320, #9631, #6138, .T. ) ;
#15239 = EDGE_LOOP ( 'NONE', ( #3225, #6700, #13717, #11550 ) ) ;
#15240 = B_SPLINE_CURVE_WITH_KNOTS ( 'NONE', 3,
 ( #3313, #2144, #3484, #5569, #9201, #9442 ),
 .UNSPECIFIED., .F., .F.,
 ( 4, 2, 4 ),
 ( 0.0002654705156154514491, 0.0005264791512502068564, 0.0007874877868849623720 ),
 .UNSPECIFIED. ) ;
#15241 = ORIENTED_EDGE ( 'NONE', *, *, #14724, .T. ) ;
#15242 = FACE_OUTER_BOUND ( 'NONE', #14158, .T. ) ;
#15243 = EDGE_CURVE ( 'NONE', #6007, #8, #11273, .T. ) ;
#15244 = CARTESIAN_POINT ( 'NONE',  ( -0.2362204724409448231, -0.02638708502139245488, 0.05905511811023622659 ) ) ;
#15245 = FACE_OUTER_BOUND ( 'NONE', #6029, .T. ) ;
#15246 =( NAMED_UNIT ( * ) SI_UNIT ( $, .STERADIAN. ) SOLID_ANGLE_UNIT ( ) );
#15247 = DIRECTION ( 'NONE',  ( 0.7632379718491706377, 0.6461174802832411190, 0.000000000000000000 ) ) ;
#15248 = DIRECTION ( 'NONE',  ( 0.000000000000000000, -1.000000000000000000, 0.000000000000000000 ) ) ;
#15249 = LINE ( 'NONE', #14302, #13870 ) ;
#15250 = DIRECTION ( 'NONE',  ( -0.5984233124757364353, -0.8011800915434477144, 0.000000000000000000 ) ) ;
#15251 = SURFACE_STYLE_USAGE ( .BOTH. , #12902 ) ;
#15252 = VERTEX_POINT ( 'NONE', #14805 ) ;
#15253 = ORIENTED_EDGE ( 'NONE', *, *, #1233, .T. ) ;
#15254 = ORIENTED_EDGE ( 'NONE', *, *, #3852, .T. ) ;
#15255 = EDGE_CURVE ( 'NONE', #10823, #11092, #13465, .T. ) ;
#15256 = EDGE_CURVE ( 'NONE', #12712, #14790, #1716, .T. ) ;
#15257 = CARTESIAN_POINT ( 'NONE',  ( -1.596030944582043976, 0.1136756404979572949, -0.04477369844321322373 ) ) ;
#15258 = DIRECTION ( 'NONE',  ( -3.075191616504334757E-15, 0.000000000000000000, 1.000000000000000000 ) ) ;
#15259 = FACE_OUTER_BOUND ( 'NONE', #5616, .T. ) ;
#15260 = CARTESIAN_POINT ( 'NONE',  ( 0.000000000000000000, 1.346456692913385877, 0.000000000000000000 ) ) ;
#15261 = CARTESIAN_POINT ( 'NONE',  ( -2.755905511811024056, -2.749515453455440905, 0.1756903148397124803 ) ) ;
#15262 = DIRECTION ( 'NONE',  ( -0.000000000000000000, 0.000000000000000000, 1.000000000000000000 ) ) ;
#15263 = DIRECTION ( 'NONE',  ( 0.000000000000000000, 0.000000000000000000, -1.000000000000000000 ) ) ;
#15264 = CARTESIAN_POINT ( 'NONE',  ( -1.923194646138151054, -2.809760929071067892, -0.1734154778929568597 ) ) ;
#15265 = ORIENTED_EDGE ( 'NONE', *, *, #1110, .F. ) ;
#15266 = FACE_OUTER_BOUND ( 'NONE', #3216, .T. ) ;
#15267 = CARTESIAN_POINT ( 'NONE',  ( -0.4339188594849095471, -0.2952755905511811330, 0.1732400634307318665 ) ) ;
#15268 = DIRECTION ( 'NONE',  ( 0.000000000000000000, -1.000000000000000000, 0.000000000000000000 ) ) ;
#15269 = DIMENSIONAL_EXPONENTS ( 1.000000000000000000, 0.000000000000000000, 0.000000000000000000, 0.000000000000000000, 0.000000000000000000, 0.000000000000000000, 0.000000000000000000 ) ;
#15270 = VERTEX_POINT ( 'NONE', #11111 ) ;
#15271 = EDGE_CURVE ( 'NONE', #2760, #6757, #6955, .T. ) ;
#15272 = ORIENTED_EDGE ( 'NONE', *, *, #8195, .T. ) ;
#15273 = ADVANCED_FACE ( 'NONE', ( #401 ), #10458, .F. ) ;
#15274 = ORIENTED_EDGE ( 'NONE', *, *, #5770, .F. ) ;
#15275 = DIRECTION ( 'NONE',  ( 0.000000000000000000, 1.000000000000000000, 0.000000000000000000 ) ) ;
#15276 = EDGE_CURVE ( 'NONE', #3617, #9786, #12858, .T. ) ;
#15277 = DIRECTION ( 'NONE',  ( 0.000000000000000000, 0.000000000000000000, 1.000000000000000000 ) ) ;
#15278 = DIRECTION ( 'NONE',  ( 5.642372883946976675E-29, -6.505213034913038437E-15, 1.000000000000000000 ) ) ;
#15279 = DIRECTION ( 'NONE',  ( -0.5000000000000004441, -0.000000000000000000, 0.8660254037844382635 ) ) ;
#15280 = ORIENTED_EDGE ( 'NONE', *, *, #9246, .T. ) ;
#15281 = CYLINDRICAL_SURFACE ( 'NONE', #8935, 0.003937007874015721089 ) ;
#15282 = EDGE_CURVE ( 'NONE', #10892, #11777, #10956, .T. ) ;
#15283 = CARTESIAN_POINT ( 'NONE',  ( -0.05905511811023622659, 1.338626482899105241, -0.5946706712680680518 ) ) ;
#15284 = CARTESIAN_POINT ( 'NONE',  ( -0.07002599089419499212, 0.1451652216336531409, 0.05905511811023622659 ) ) ;
#15285 = DIRECTION ( 'NONE',  ( 0.000000000000000000, -1.000000000000000000, 0.000000000000000000 ) ) ;
#15286 = ORIENTED_EDGE ( 'NONE', *, *, #1071, .F. ) ;
#15287 = DIRECTION ( 'NONE',  ( -0.8660254037844394848, 0.000000000000000000, 0.4999999999999985567 ) ) ;
#15288 = VERTEX_POINT ( 'NONE', #7673 ) ;
#15289 = EDGE_LOOP ( 'NONE', ( #1991, #13037, #14227, #7382 ) ) ;
#15290 = ORIENTED_EDGE ( 'NONE', *, *, #5938, .T. ) ;
#15291 = PRODUCT_DEFINITION_SHAPE ( 'NONE', 'NONE',  #6282 ) ;
#15292 = EDGE_LOOP ( 'NONE', ( #7730, #1498, #8276, #3192, #1584, #12571, #5621, #10640 ) ) ;
#15293 = EDGE_CURVE ( 'NONE', #13738, #4902, #8470, .T. ) ;
#15294 = DIRECTION ( 'NONE',  ( 0.8660254037844395958, 0.000000000000000000, -0.4999999999999982236 ) ) ;
#15295 = CARTESIAN_POINT ( 'NONE',  ( -0.4586614173228359959, -0.1023622047244094474, 0.3875520507749251053 ) ) ;
#15296 = CARTESIAN_POINT ( 'NONE',  ( -0.03608642540485051259, 0.1707537476062188919, -0.01804586331702247651 ) ) ;
#15297 = CARTESIAN_POINT ( 'NONE',  ( -0.5905511811023621549, 2.448818897637795367, -0.04724409448818898266 ) ) ;
#15298 = CONTEXT_DEPENDENT_SHAPE_REPRESENTATION ( #13407, #9951 ) ;
#15299 = DIRECTION ( 'NONE',  ( 1.172998894335282758E-16, -0.2873478855663456066, 0.9578262852211513190 ) ) ;
#15300 = CARTESIAN_POINT ( 'NONE',  ( -0.1023622047242992161, -0.2952755905511811330, -0.4190977005962941981 ) ) ;
#15301 = EDGE_CURVE ( 'NONE', #1810, #5085, #3706, .T. ) ;
#15302 = ORIENTED_EDGE ( 'NONE', *, *, #10486, .F. ) ;
#15303 = DIRECTION ( 'NONE',  ( -0.8660254037844428154, 0.000000000000000000, -0.4999999999999926725 ) ) ;
#15304 = EDGE_CURVE ( 'NONE', #5535, #5050, #474, .T. ) ;
#15305 = DIRECTION ( 'NONE',  ( 3.973232667114494807E-16, -0.000000000000000000, -1.000000000000000000 ) ) ;
#15306 = CARTESIAN_POINT ( 'NONE',  ( -0.1804058482824385523, -0.4881889763779528324, -0.1041573650692488306 ) ) ;
#15307 = ORIENTED_EDGE ( 'NONE', *, *, #11224, .T. ) ;
#15308 = ADVANCED_BREP_SHAPE_REPRESENTATION ( '', ( #4199, #11481 ), #7464 ) ;
#15309 = ORIENTED_EDGE ( 'NONE', *, *, #12662, .T. ) ;
#15310 = CARTESIAN_POINT ( 'NONE',  ( -0.5433070866141463950, -0.4881889763779528324, 0.2409414509217019384 ) ) ;
#15311 = ORIENTED_EDGE ( 'NONE', *, *, #2960, .F. ) ;
#15312 = ORIENTED_EDGE ( 'NONE', *, *, #4359, .T. ) ;
#15313 = ORIENTED_EDGE ( 'NONE', *, *, #6972, .F. ) ;
#15314 = CARTESIAN_POINT ( 'NONE',  ( -2.087029306903609438, -1.707904051420249480, 0.08366141732283424726 ) ) ;
#15315 = FACE_OUTER_BOUND ( 'NONE', #3302, .T. ) ;
#15316 = CARTESIAN_POINT ( 'NONE',  ( -1.919797936996253451, -2.887775577793183945, 0.1348761084896591966 ) ) ;
#15317 = DIRECTION ( 'NONE',  ( 1.000000000000000000, 0.000000000000000000, 0.000000000000000000 ) ) ;
#15318 = FACE_BOUND ( 'NONE', #2761, .T. ) ;
#15319 = DIRECTION ( 'NONE',  ( -0.000000000000000000, 1.000000000000000000, -0.000000000000000000 ) ) ;
#15320 = DIRECTION ( 'NONE',  ( -0.000000000000000000, -1.000000000000000000, -0.000000000000000000 ) ) ;
#15321 = PRODUCT_DEFINITION ( 'UNKNOWN', '', #5106, #12698 ) ;
#15322 = DIRECTION ( 'NONE',  ( -0.000000000000000000, -0.000000000000000000, -1.000000000000000000 ) ) ;
#15323 = CARTESIAN_POINT ( 'NONE',  ( 0.4788739157331329821, -0.1023622047244094474, 0.3446689608323529885 ) ) ;
#15324 = CARTESIAN_POINT ( 'NONE',  ( -2.086995670982084050, -1.707489817804680232, -0.08366141732283374766 ) ) ;
#15325 = DIRECTION ( 'NONE',  ( 0.000000000000000000, 1.000000000000000000, 2.183568011719057743E-16 ) ) ;
#15326 = VERTEX_POINT ( 'NONE', #9775 ) ;
#15327 = ORIENTED_EDGE ( 'NONE', *, *, #9619, .F. ) ;
#15328 = EDGE_LOOP ( 'NONE', ( #2709, #10692, #12654, #10581 ) ) ;
#15329 = ORIENTED_EDGE ( 'NONE', *, *, #2599, .F. ) ;
#15330 = DIRECTION ( 'NONE',  ( -0.000000000000000000, -1.000000000000000000, -0.000000000000000000 ) ) ;
#15331 = CARTESIAN_POINT ( 'NONE',  ( -0.06997329305368624186, 0.1451708428228431214, 0.05905511811023621271 ) ) ;
#15332 = ADVANCED_FACE ( 'NONE', ( #8578 ), #12969, .F. ) ;
#15333 = CARTESIAN_POINT ( 'NONE',  ( 0.000000000000000000, 0.07874015748031495954, 0.000000000000000000 ) ) ;
#15334 = CARTESIAN_POINT ( 'NONE',  ( 0.000000000000000000, 0.5905511811023621549, -0.7007874015748031260 ) ) ;
#15335 = VECTOR ( 'NONE', #1475, 39.37007874015748143 ) ;
#15336 = FACE_BOUND ( 'NONE', #10875, .T. ) ;
#15337 = EDGE_CURVE ( 'NONE', #7829, #12817, #2465, .T. ) ;
#15338 = VERTEX_POINT ( 'NONE', #7186 ) ;
#15339 = DIRECTION ( 'NONE',  ( 0.000000000000000000, 0.000000000000000000, -1.000000000000000000 ) ) ;
#15340 = VECTOR ( 'NONE', #11176, 39.37007874015748143 ) ;
#15341 = CARTESIAN_POINT ( 'NONE',  ( 6.846450609406462919E-17, 0.3464566929133857109, 0.5590551181102362266 ) ) ;
#15342 = CYLINDRICAL_SURFACE ( 'NONE', #159, 0.003937007874015758385 ) ;
#15343 = CIRCLE ( 'NONE', #9839, 0.007874015748031516770 ) ;
#15344 = VERTEX_POINT ( 'NONE', #12046 ) ;
#15345 = EDGE_CURVE ( 'NONE', #9943, #14086, #4462, .T. ) ;
#15346 = ORIENTED_EDGE ( 'NONE', *, *, #14226, .T. ) ;
#15347 = ORIENTED_EDGE ( 'NONE', *, *, #2078, .F. ) ;
#15348 = AXIS2_PLACEMENT_3D ( 'NONE', #6863, #10551, #3438 ) ;
#15349 = VECTOR ( 'NONE', #6695, 39.37007874015748143 ) ;
#15350 = CIRCLE ( 'NONE', #6078, 0.003937007874015758385 ) ;
#15351 = AXIS2_PLACEMENT_3D ( 'NONE', #7247, #6049, #5910 ) ;
#15352 = ADVANCED_FACE ( 'NONE', ( #3740 ), #12274, .T. ) ;
#15353 = SPHERICAL_SURFACE ( 'NONE', #7612, 0.003937007874015747977 ) ;
#15354 = CARTESIAN_POINT ( 'NONE',  ( -1.928486289398714915, -2.940034385472957812, 0.05833844333314246872 ) ) ;
#15355 = CARTESIAN_POINT ( 'NONE',  ( 0.2353927734920605308, -0.09842519685039370636, 0.06771310446505662828 ) ) ;
#15356 = CARTESIAN_POINT ( 'NONE',  ( -1.888479416392070398, -2.900872351736208277, 0.1227802583590561630 ) ) ;
#15357 = EDGE_CURVE ( 'NONE', #6019, #11619, #2717, .T. ) ;
#15358 = EDGE_LOOP ( 'NONE', ( #14504, #9636, #8595, #1318 ) ) ;
#15359 = CARTESIAN_POINT ( 'NONE',  ( 0.000000000000000000, 1.035433070866142113, 0.000000000000000000 ) ) ;
#15360 = CARTESIAN_POINT ( 'NONE',  ( 0.000000000000000000, -0.003937007874015747977, -0.5870514566507987197 ) ) ;
#15361 = CIRCLE ( 'NONE', #6075, 0.01968503937007875723 ) ;
#15362 = VECTOR ( 'NONE', #2048, 39.37007874015748143 ) ;
#15363 = DIRECTION ( 'NONE',  ( 0.4999999999999827915, -0.000000000000000000, -0.8660254037844488106 ) ) ;
#15364 = CARTESIAN_POINT ( 'NONE',  ( -1.607606114292111199, 0.09732815221480028978, 0.07874015748031495954 ) ) ;
#15365 = ORIENTED_EDGE ( 'NONE', *, *, #7517, .F. ) ;
#15366 = VECTOR ( 'NONE', #1369, 39.37007874015748143 ) ;
#15367 = EDGE_CURVE ( 'NONE', #13986, #13529, #12981, .T. ) ;
#15368 = CARTESIAN_POINT ( 'NONE',  ( 1.181102362204724310, 0.1279527559055117225, -0.02559055118110236185 ) ) ;
#15369 = CIRCLE ( 'NONE', #14603, 0.6692913385826770867 ) ;
#15370 = B_SPLINE_CURVE_WITH_KNOTS ( 'NONE', 3,
 ( #2094, #9390, #9236, #8282, #14169, #5759, #12993, #1950, #13934, #15188 ),
 .UNSPECIFIED., .F., .F.,
 ( 4, 2, 2, 2, 4 ),
 ( 0.000000000000000000, 0.0006596926164930297203, 0.001319385232986059441, 0.001979077849479089161, 0.002638770465972118881 ),
 .UNSPECIFIED. ) ;
#15371 = ORIENTED_EDGE ( 'NONE', *, *, #12961, .T. ) ;
#15372 = ORIENTED_EDGE ( 'NONE', *, *, #14722, .F. ) ;
#15373 = DIRECTION ( 'NONE',  ( 0.000000000000000000, 0.000000000000000000, -1.000000000000000000 ) ) ;
#15374 = FACE_OUTER_BOUND ( 'NONE', #5598, .T. ) ;
#15375 = VECTOR ( 'NONE', #8500, 39.37007874015748143 ) ;
#15376 = VECTOR ( 'NONE', #12951, 39.37007874015748143 ) ;
#15377 = AXIS2_PLACEMENT_3D ( 'NONE', #10496, #11587, #640 ) ;
#15378 = CARTESIAN_POINT ( 'NONE',  ( -1.607606114292111643, 0.09732815221480056733, -0.07528735249397262852 ) ) ;
#15379 = CARTESIAN_POINT ( 'NONE',  ( -0.07874015748031494566, 0.1685051786281938357, -0.03937007874015750752 ) ) ;
#15380 = VECTOR ( 'NONE', #14252, 39.37007874015748143 ) ;
#15381 = DIRECTION ( 'NONE',  ( 1.000000000000000000, -0.000000000000000000, -0.000000000000000000 ) ) ;
#15382 = AXIS2_PLACEMENT_3D ( 'NONE', #6439, #7770, #13973 ) ;
#15383 = DIRECTION ( 'NONE',  ( 1.000000000000000000, 0.000000000000000000, 3.476578583725179813E-16 ) ) ;
#15385 = ORIENTED_EDGE ( 'NONE', *, *, #3755, .F. ) ;
#15384 = PRODUCT_DEFINITION_FORMATION_WITH_SPECIFIED_SOURCE ( 'ANY', '', #1908, .NOT_KNOWN. ) ;
#15386 = DIRECTION ( 'NONE',  ( 0.000000000000000000, -0.000000000000000000, 1.000000000000000000 ) ) ;
#15387 = DIRECTION ( 'NONE',  ( -0.8660254037844432595, 0.000000000000000000, -0.4999999999999918954 ) ) ;
#15388 = CARTESIAN_POINT ( 'NONE',  ( 0.05905511811023622659, 1.043263280880422528, -0.5946706712680680518 ) ) ;
#15389 = EDGE_CURVE ( 'NONE', #7774, #13558, #2966, .T. ) ;
#15390 = VECTOR ( 'NONE', #10360, 39.37007874015748143 ) ;
#15391 = AXIS2_PLACEMENT_3D ( 'NONE', #10173, #7563, #9002 ) ;
#15392 = AXIS2_PLACEMENT_3D ( 'NONE', #9120, #6998, #10601 ) ;
#15393 = ORIENTED_EDGE ( 'NONE', *, *, #2809, .T. ) ;
#15394 = DIRECTION ( 'NONE',  ( -0.5000000000000002220, 0.000000000000000000, -0.8660254037844384856 ) ) ;
#15395 = VERTEX_POINT ( 'NONE', #1243 ) ;
#15396 = VECTOR ( 'NONE', #3454, 39.37007874015748143 ) ;
#15397 = ORIENTED_EDGE ( 'NONE', *, *, #12900, .T. ) ;
#15398 = FACE_OUTER_BOUND ( 'NONE', #2604, .T. ) ;
#15399 = EDGE_CURVE ( 'NONE', #5085, #12689, #6060, .T. ) ;
#15400 = ORIENTED_EDGE ( 'NONE', *, *, #3861, .F. ) ;
#15401 = SPHERICAL_SURFACE ( 'NONE', #4878, 0.003937007874015747977 ) ;
#15402 = DIRECTION ( 'NONE',  ( -0.000000000000000000, 1.000000000000000000, 0.000000000000000000 ) ) ;
#15403 = DIRECTION ( 'NONE',  ( 0.4999999999999798495, 0.000000000000000000, -0.8660254037844501429 ) ) ;
#15404 = DIRECTION ( 'NONE',  ( 0.000000000000000000, 0.000000000000000000, 1.000000000000000000 ) ) ;
#15405 = VECTOR ( 'NONE', #4776, 39.37007874015748143 ) ;
#15406 = FILL_AREA_STYLE_COLOUR ( '', #6849 ) ;
#15407 = CIRCLE ( 'NONE', #13150, 0.003937007874015749712 ) ;
#15408 = DIRECTION ( 'NONE',  ( -1.224646799147352961E-16, 0.000000000000000000, -1.000000000000000000 ) ) ;
#15409 = CARTESIAN_POINT ( 'NONE',  ( 0.1734555655881918346, -0.4881889763779528324, 0.1728816592724491952 ) ) ;
#15410 = CYLINDRICAL_SURFACE ( 'NONE', #8367, 0.003937007874015724558 ) ;
#15411 = AXIS2_PLACEMENT_3D ( 'NONE', #2972, #12685, #13535 ) ;
#15412 = DIRECTION ( 'NONE',  ( 1.000000000000000000, 0.000000000000000000, 0.000000000000000000 ) ) ;
#15413 = ORIENTED_EDGE ( 'NONE', *, *, #8473, .T. ) ;
#15414 = VERTEX_POINT ( 'NONE', #10782 ) ;
#15415 = CIRCLE ( 'NONE', #8651, 0.1653543307086614012 ) ;
#15416 = VERTEX_POINT ( 'NONE', #5128 ) ;
#15417 = AXIS2_PLACEMENT_3D ( 'NONE', #1479, #13293, #5048 ) ;
#15418 = AXIS2_PLACEMENT_3D ( 'NONE', #10047, #10214, #6505 ) ;
#15419 = EDGE_LOOP ( 'NONE', ( #3925, #7801 ) ) ;
#15420 = EDGE_CURVE ( 'NONE', #13926, #5735, #2716, .T. ) ;
#15421 = AXIS2_PLACEMENT_3D ( 'NONE', #12049, #3894, #121 ) ;
#15422 = CARTESIAN_POINT ( 'NONE',  ( 0.06011003619072806392, -0.09842519685039370636, -0.2337756660697248301 ) ) ;
#15423 = CARTESIAN_POINT ( 'NONE',  ( 0.000000000000000000, 0.000000000000000000, 0.000000000000000000 ) ) ;
#15424 = DIRECTION ( 'NONE',  ( 1.000000000000000000, 0.000000000000000000, 0.000000000000000000 ) ) ;
#15425 = FACE_OUTER_BOUND ( 'NONE', #6554, .T. ) ;
#15426 = CIRCLE ( 'NONE', #11678, 0.003937007874015721089 ) ;
#15427 = CARTESIAN_POINT ( 'NONE',  ( 0.05905511811023622659, 1.043307086614173373, -0.5952259495879739237 ) ) ;
#15428 = EDGE_LOOP ( 'NONE', ( #5146, #1355, #12775, #812 ) ) ;
#15429 = CARTESIAN_POINT ( 'NONE',  ( -0.1259842519685039353, 2.440944881889763884, -0.04724409448818898266 ) ) ;
#15430 = LINE ( 'NONE', #8048, #2607 ) ;
#15431 = DIRECTION ( 'NONE',  ( 0.5000000000000035527, -0.000000000000000000, -0.8660254037844365982 ) ) ;
#15432 = CIRCLE ( 'NONE', #8921, 0.1574803149606299191 ) ;
#15433 = ORIENTED_EDGE ( 'NONE', *, *, #13039, .T. ) ;
#15434 = ORIENTED_EDGE ( 'NONE', *, *, #3753, .F. ) ;
#15435 = ORIENTED_EDGE ( 'NONE', *, *, #1981, .T. ) ;
#15436 = VECTOR ( 'NONE', #6999, 39.37007874015748143 ) ;
#15437 = ADVANCED_FACE ( 'NONE', ( #2545 ), #9733, .T. ) ;
#15438 = CARTESIAN_POINT ( 'NONE',  ( -1.987684632567998877, -2.764755981110976091, 0.1771653543306854761 ) ) ;
#15439 = AXIS2_PLACEMENT_3D ( 'NONE', #8238, #13012, #3226 ) ;
#15440 = EDGE_CURVE ( 'NONE', #8101, #2525, #4723, .T. ) ;
#15441 = CARTESIAN_POINT ( 'NONE',  ( 1.181102362204724310, 4.044111181948214319E-16, 0.02559055118110236185 ) ) ;
#15442 = DIRECTION ( 'NONE',  ( -0.8660254037844385966, 0.000000000000000000, -0.5000000000000001110 ) ) ;
#15443 = DIRECTION ( 'NONE',  ( 0.000000000000000000, 1.000000000000000000, 0.000000000000000000 ) ) ;
#15444 = CARTESIAN_POINT ( 'NONE',  ( -1.949178430106353499, -2.798437798732091419, 0.1753388726975497469 ) ) ;
#15445 = ORIENTED_EDGE ( 'NONE', *, *, #4954, .F. ) ;
#15446 = FACE_OUTER_BOUND ( 'NONE', #6021, .T. ) ;
#15447 = DIRECTION ( 'NONE',  ( 1.000000000000000000, 0.000000000000000000, 0.000000000000000000 ) ) ;
#15448 = CIRCLE ( 'NONE', #10704, 0.003937007874015758385 ) ;
#15449 = DIRECTION ( 'NONE',  ( -0.8660254037844428154, 0.000000000000000000, -0.4999999999999926725 ) ) ;
#15450 = DIRECTION ( 'NONE',  ( 0.000000000000000000, 1.000000000000000000, 0.000000000000000000 ) ) ;
#15451 = ORIENTED_EDGE ( 'NONE', *, *, #7757, .F. ) ;
#15452 = TOROIDAL_SURFACE ( 'NONE', #4929, 0.2303149606299203511, 0.01968503937007873988 ) ;
#15453 = ORIENTED_EDGE ( 'NONE', *, *, #7248, .F. ) ;
#15454 = ORIENTED_EDGE ( 'NONE', *, *, #8508, .F. ) ;
#15455 = AXIS2_PLACEMENT_3D ( 'NONE', #4867, #9666, #12166 ) ;
#15456 = EDGE_CURVE ( 'NONE', #7829, #13509, #6968, .T. ) ;
#15457 = DIRECTION ( 'NONE',  ( -0.5000000000000035527, 0.000000000000000000, 0.8660254037844365982 ) ) ;
#15458 = DIRECTION ( 'NONE',  ( 0.4999999999999979461, 0.000000000000000000, 0.8660254037844398178 ) ) ;
#15459 = DIRECTION ( 'NONE',  ( -0.4999999999999966693, 0.000000000000000000, 0.8660254037844405950 ) ) ;
#15460 = AXIS2_PLACEMENT_3D ( 'NONE', #9054, #7548, #523 ) ;
#15461 = EDGE_CURVE ( 'NONE', #11838, #10253, #4910, .T. ) ;
#15462 = CARTESIAN_POINT ( 'NONE',  ( -1.417133371508829898, -0.01083197275114198763, 0.06860104880227285706 ) ) ;
#15463 = DIRECTION ( 'NONE',  ( -0.000000000000000000, -1.000000000000000000, -0.000000000000000000 ) ) ;
#15464 = CONTEXT_DEPENDENT_SHAPE_REPRESENTATION ( #4591, #3426 ) ;
#15465 = CARTESIAN_POINT ( 'NONE',  ( 0.000000000000000000, 0.04724409448818898960, -0.5433070866141731514 ) ) ;
#15466 = CIRCLE ( 'NONE', #7201, 0.5905511811023621549 ) ;
#15467 = CARTESIAN_POINT ( 'NONE',  ( -1.185322955811905166, 0.3350001079061992182, 0.05695403563116168549 ) ) ;
#15468 = EDGE_LOOP ( 'NONE', ( #1674, #6232, #15286, #11989, #3291 ) ) ;
#15469 = CARTESIAN_POINT ( 'NONE',  ( 0.000000000000000000, 2.393700787401575436, 0.000000000000000000 ) ) ;
#15470 = NEXT_ASSEMBLY_USAGE_OCCURRENCE ( 'NAUO1', ' ', ' ', #3539, #6282, $ ) ;
#15471 = NEXT_ASSEMBLY_USAGE_OCCURRENCE ( 'NAUO2', ' ', ' ', #3539, #9773, $ ) ;
#15472 = NEXT_ASSEMBLY_USAGE_OCCURRENCE ( 'NAUO3', ' ', ' ', #3539, #15321, $ ) ;
#15473 = NEXT_ASSEMBLY_USAGE_OCCURRENCE ( 'NAUO4', ' ', ' ', #3539, #561, $ ) ;
#15474 = NEXT_ASSEMBLY_USAGE_OCCURRENCE ( 'NAUO5', ' ', ' ', #3539, #15321, $ ) ;
#15475 = NEXT_ASSEMBLY_USAGE_OCCURRENCE ( 'NAUO6', ' ', ' ', #3539, #3339, $ ) ;
#15476 = NEXT_ASSEMBLY_USAGE_OCCURRENCE ( 'NAUO7', ' ', ' ', #3539, #3339, $ ) ;
#15477 = NEXT_ASSEMBLY_USAGE_OCCURRENCE ( 'NAUO8', ' ', ' ', #3539, #3339, $ ) ;
#15478 = NEXT_ASSEMBLY_USAGE_OCCURRENCE ( 'NAUO9', ' ', ' ', #3539, #6099, $ ) ;
#15479 = NEXT_ASSEMBLY_USAGE_OCCURRENCE ( 'NAUO10', ' ', ' ', #3539, #6099, $ ) ;
#15480 = NEXT_ASSEMBLY_USAGE_OCCURRENCE ( 'NAUO11', ' ', ' ', #3539, #6099, $ ) ;
#15481 = NEXT_ASSEMBLY_USAGE_OCCURRENCE ( 'NAUO12', ' ', ' ', #3539, #6099, $ ) ;
#15482 = NEXT_ASSEMBLY_USAGE_OCCURRENCE ( 'NAUO13', ' ', ' ', #3539, #6099, $ ) ;
#15483 = NEXT_ASSEMBLY_USAGE_OCCURRENCE ( 'NAUO14', ' ', ' ', #3539, #6099, $ ) ;
#15484 = NEXT_ASSEMBLY_USAGE_OCCURRENCE ( 'NAUO15', ' ', ' ', #3539, #6099, $ ) ;
#15485 = NEXT_ASSEMBLY_USAGE_OCCURRENCE ( 'NAUO16', ' ', ' ', #3539, #6099, $ ) ;
#15486 = NEXT_ASSEMBLY_USAGE_OCCURRENCE ( 'NAUO17', ' ', ' ', #3539, #6099, $ ) ;
#15487 = NEXT_ASSEMBLY_USAGE_OCCURRENCE ( 'NAUO18', ' ', ' ', #3539, #3339, $ ) ;
#15488 = NEXT_ASSEMBLY_USAGE_OCCURRENCE ( 'NAUO19', ' ', ' ', #3539, #3339, $ ) ;
#15489 = NEXT_ASSEMBLY_USAGE_OCCURRENCE ( 'NAUO20', ' ', ' ', #3539, #3339, $ ) ;
#15490 = NEXT_ASSEMBLY_USAGE_OCCURRENCE ( 'NAUO21', ' ', ' ', #3539, #3339, $ ) ;
#15491 = NEXT_ASSEMBLY_USAGE_OCCURRENCE ( 'NAUO22', ' ', ' ', #3539, #3339, $ ) ;
#15492 = NEXT_ASSEMBLY_USAGE_OCCURRENCE ( 'NAUO23', ' ', ' ', #3539, #3339, $ ) ;
#15493 = NEXT_ASSEMBLY_USAGE_OCCURRENCE ( 'NAUO24', ' ', ' ', #3539, #15321, $ ) ;
#15494 = NEXT_ASSEMBLY_USAGE_OCCURRENCE ( 'NAUO25', ' ', ' ', #3539, #15321, $ ) ;
#15495 = NEXT_ASSEMBLY_USAGE_OCCURRENCE ( 'NAUO26', ' ', ' ', #3539, #15321, $ ) ;
#15496 = NEXT_ASSEMBLY_USAGE_OCCURRENCE ( 'NAUO27', ' ', ' ', #3539, #15321, $ ) ;
#15497 = NEXT_ASSEMBLY_USAGE_OCCURRENCE ( 'NAUO28', ' ', ' ', #3539, #561, $ ) ;
#15498 = NEXT_ASSEMBLY_USAGE_OCCURRENCE ( 'NAUO29', ' ', ' ', #3539, #561, $ ) ;
#15499=COLOUR_RGB('Dark Blue',0.08,0.2,0.34);
#15500=FILL_AREA_STYLE_COLOUR('',#15499);
#15501=FILL_AREA_STYLE('',(#15500));
#15502=SURFACE_STYLE_FILL_AREA(#15501);
#15503=SURFACE_SIDE_STYLE('',(#15502));
#15504=SURFACE_STYLE_USAGE(.BOTH.,#15503);
#15505=PRESENTATION_STYLE_ASSIGNMENT((#15504));
#15506=COLOUR_RGB('Light Blue',0.38,0.62,0.78);
#15507=FILL_AREA_STYLE_COLOUR('',#15506);
#15508=FILL_AREA_STYLE('',(#15507));
#15509=SURFACE_STYLE_FILL_AREA(#15508);
#15510=SURFACE_SIDE_STYLE('',(#15509));
#15511=SURFACE_STYLE_USAGE(.BOTH.,#15510);
#15512=PRESENTATION_STYLE_ASSIGNMENT((#15511));
#15513=COLOUR_RGB('Sky Blue',0.24,0.69,0.87);
#15514=FILL_AREA_STYLE_COLOUR('',#15513);
#15515=FILL_AREA_STYLE('',(#15514));
#15516=SURFACE_STYLE_FILL_AREA(#15515);
#15517=SURFACE_SIDE_STYLE('',(#15516));
#15518=SURFACE_STYLE_USAGE(.BOTH.,#15517);
#15519=PRESENTATION_STYLE_ASSIGNMENT((#15518));
#15520=COLOUR_RGB('Grey',0.48,0.52,0.57);
#15521=FILL_AREA_STYLE_COLOUR('',#15520);
#15522=FILL_AREA_STYLE('',(#15521));
#15523=SURFACE_STYLE_FILL_AREA(#15522);
#15524=SURFACE_SIDE_STYLE('',(#15523));
#15525=SURFACE_STYLE_USAGE(.BOTH.,#15524);
#15526=PRESENTATION_STYLE_ASSIGNMENT((#15525));
#15527=COLOUR_RGB('Black',0.12,0.14,0.17);
#15528=FILL_AREA_STYLE_COLOUR('',#15527);
#15529=FILL_AREA_STYLE('',(#15528));
#15530=SURFACE_STYLE_FILL_AREA(#15529);
#15531=SURFACE_SIDE_STYLE('',(#15530));
#15532=SURFACE_STYLE_USAGE(.BOTH.,#15531);
#15533=PRESENTATION_STYLE_ASSIGNMENT((#15532));
#15534=COLOUR_RGB('Off White',0.89,0.88,0.83);
#15535=FILL_AREA_STYLE_COLOUR('',#15534);
#15536=FILL_AREA_STYLE('',(#15535));
#15537=SURFACE_STYLE_FILL_AREA(#15536);
#15538=SURFACE_SIDE_STYLE('',(#15537));
#15539=SURFACE_STYLE_USAGE(.BOTH.,#15538);
#15540=PRESENTATION_STYLE_ASSIGNMENT((#15539));
ENDSEC;
END-ISO-10303-21;
